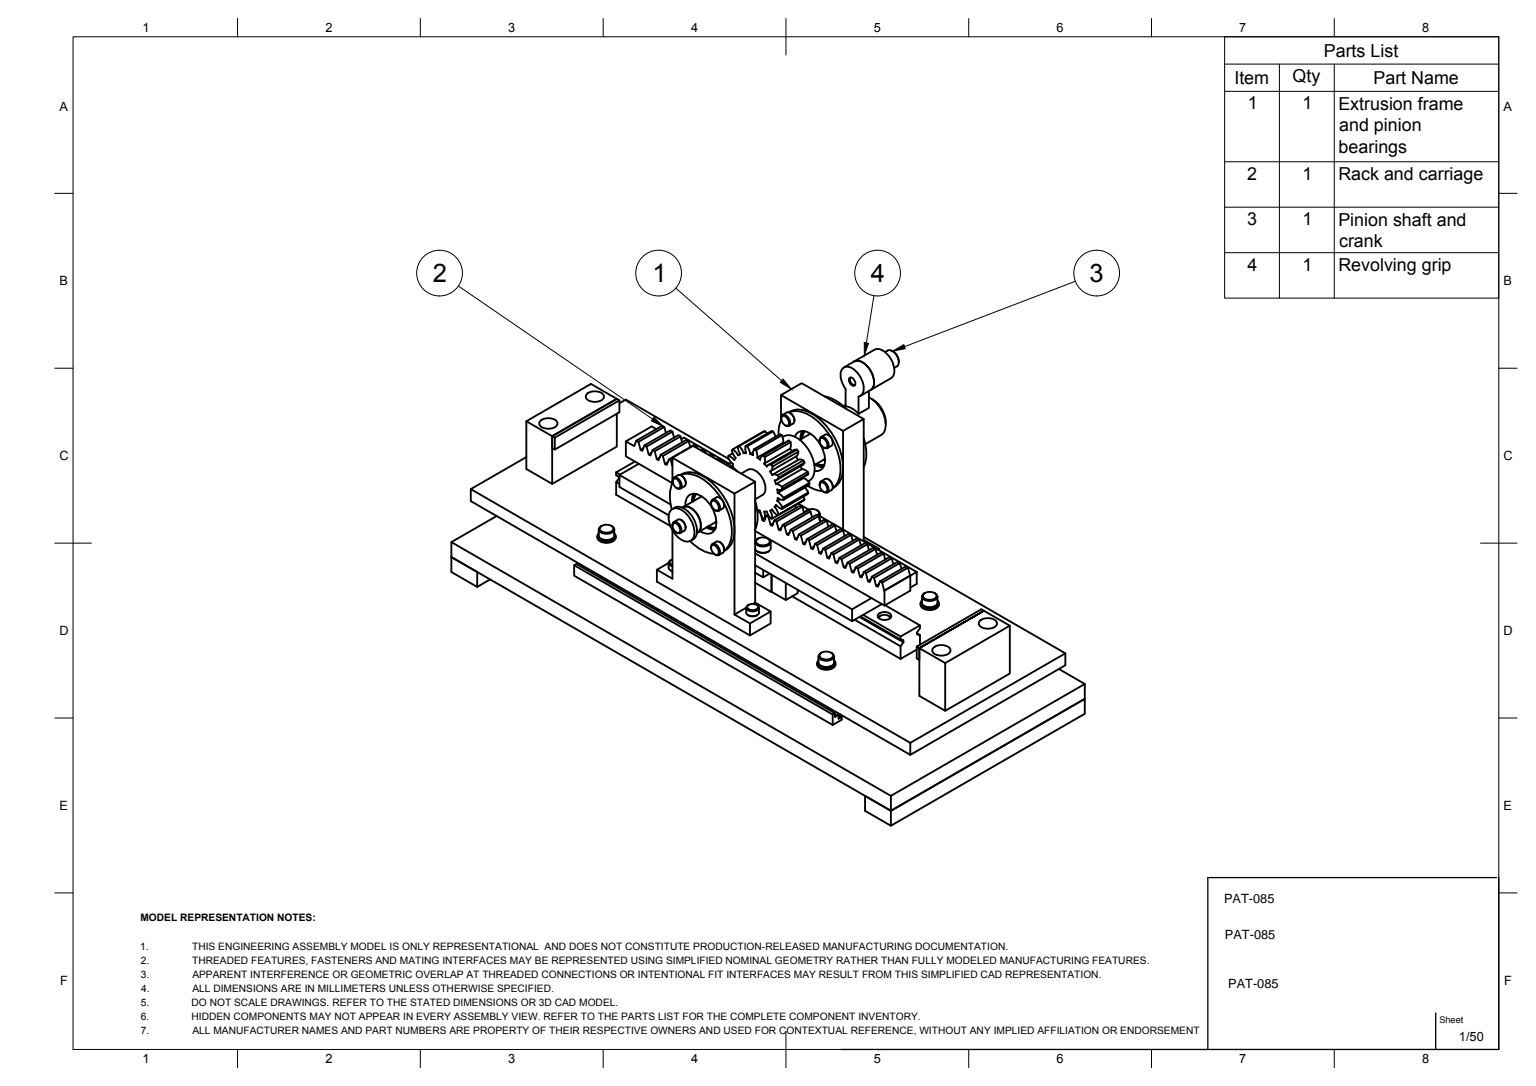
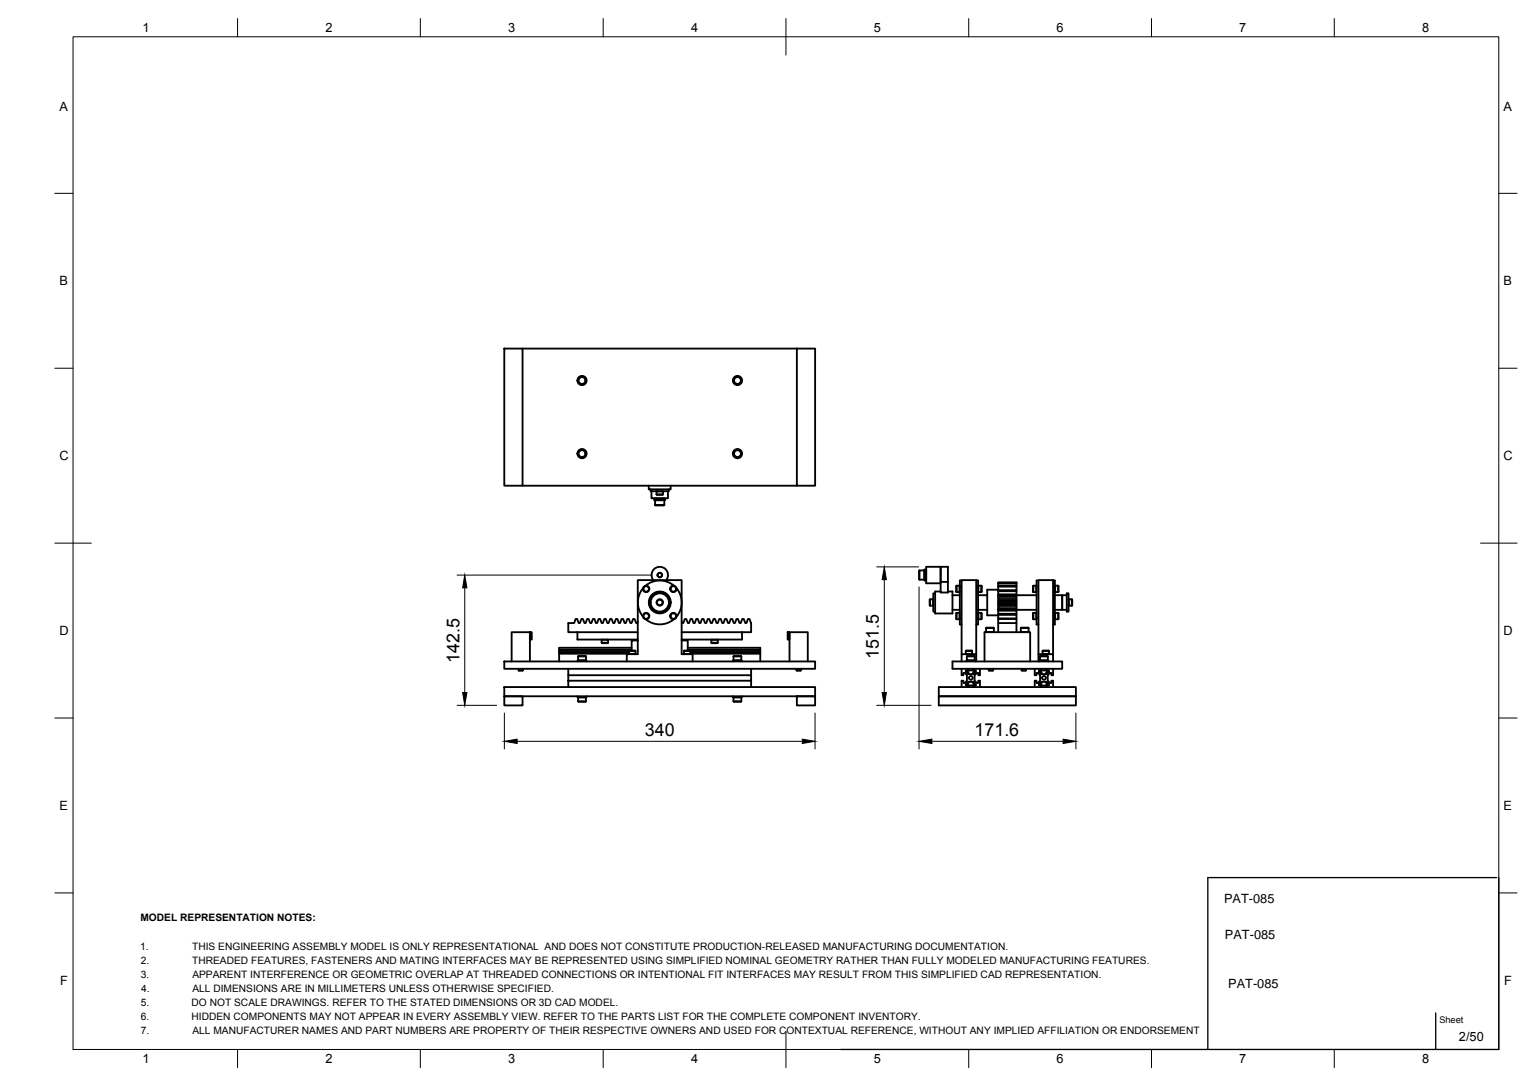
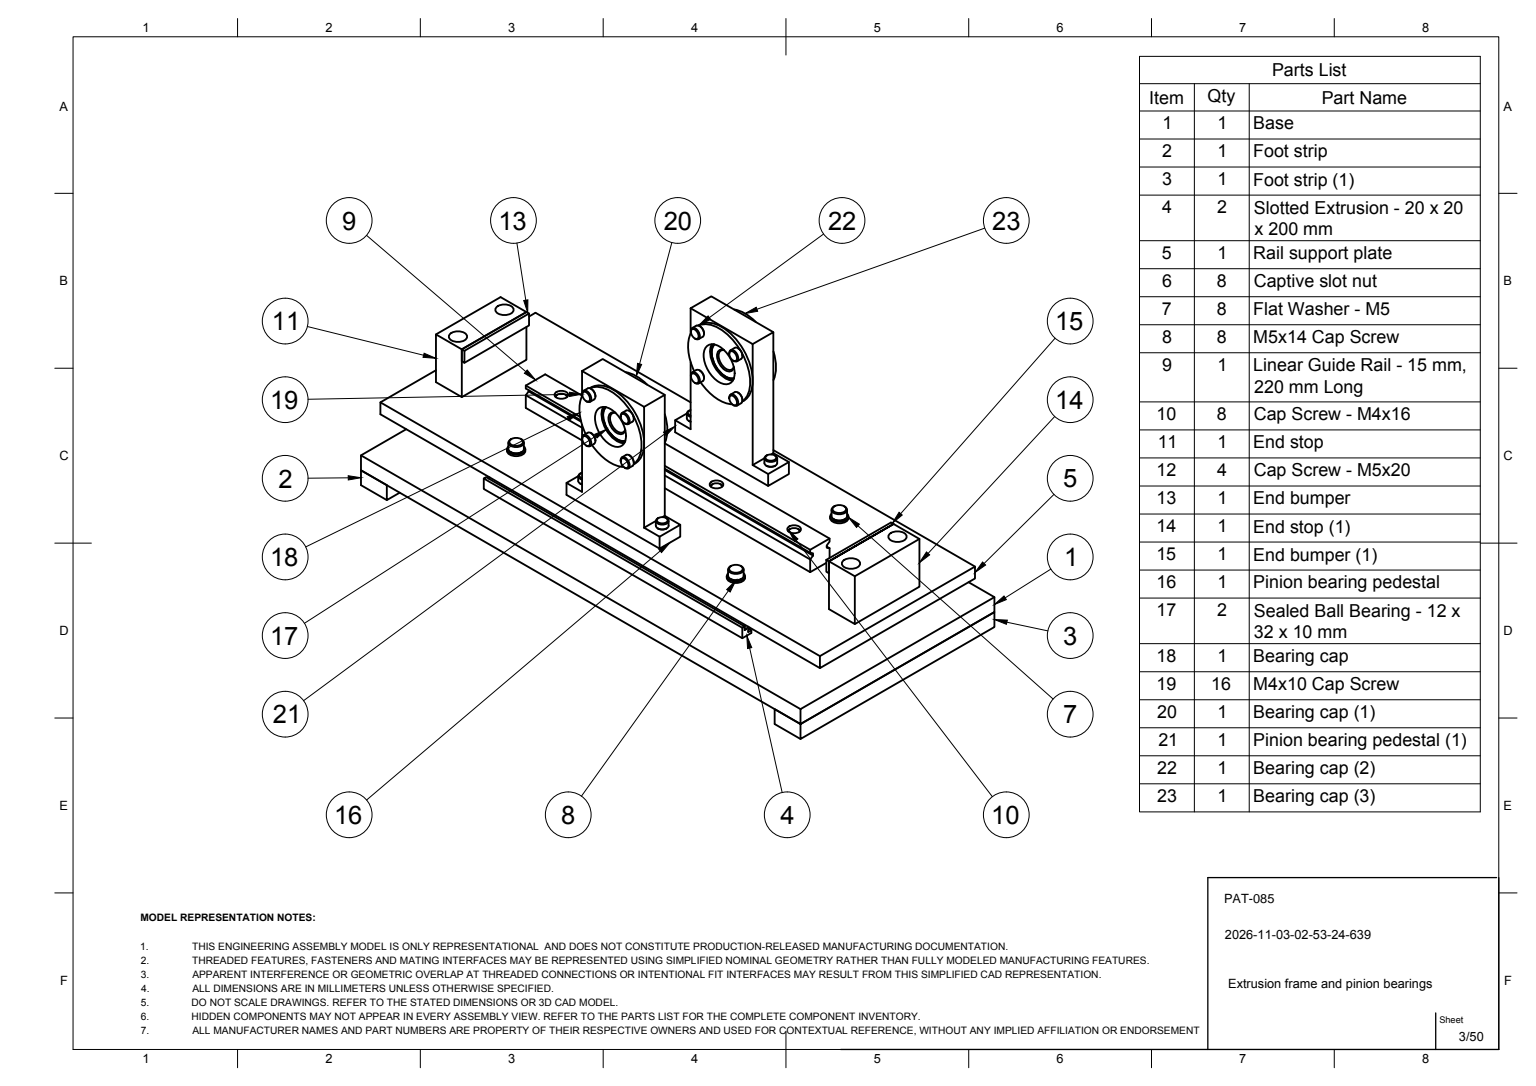
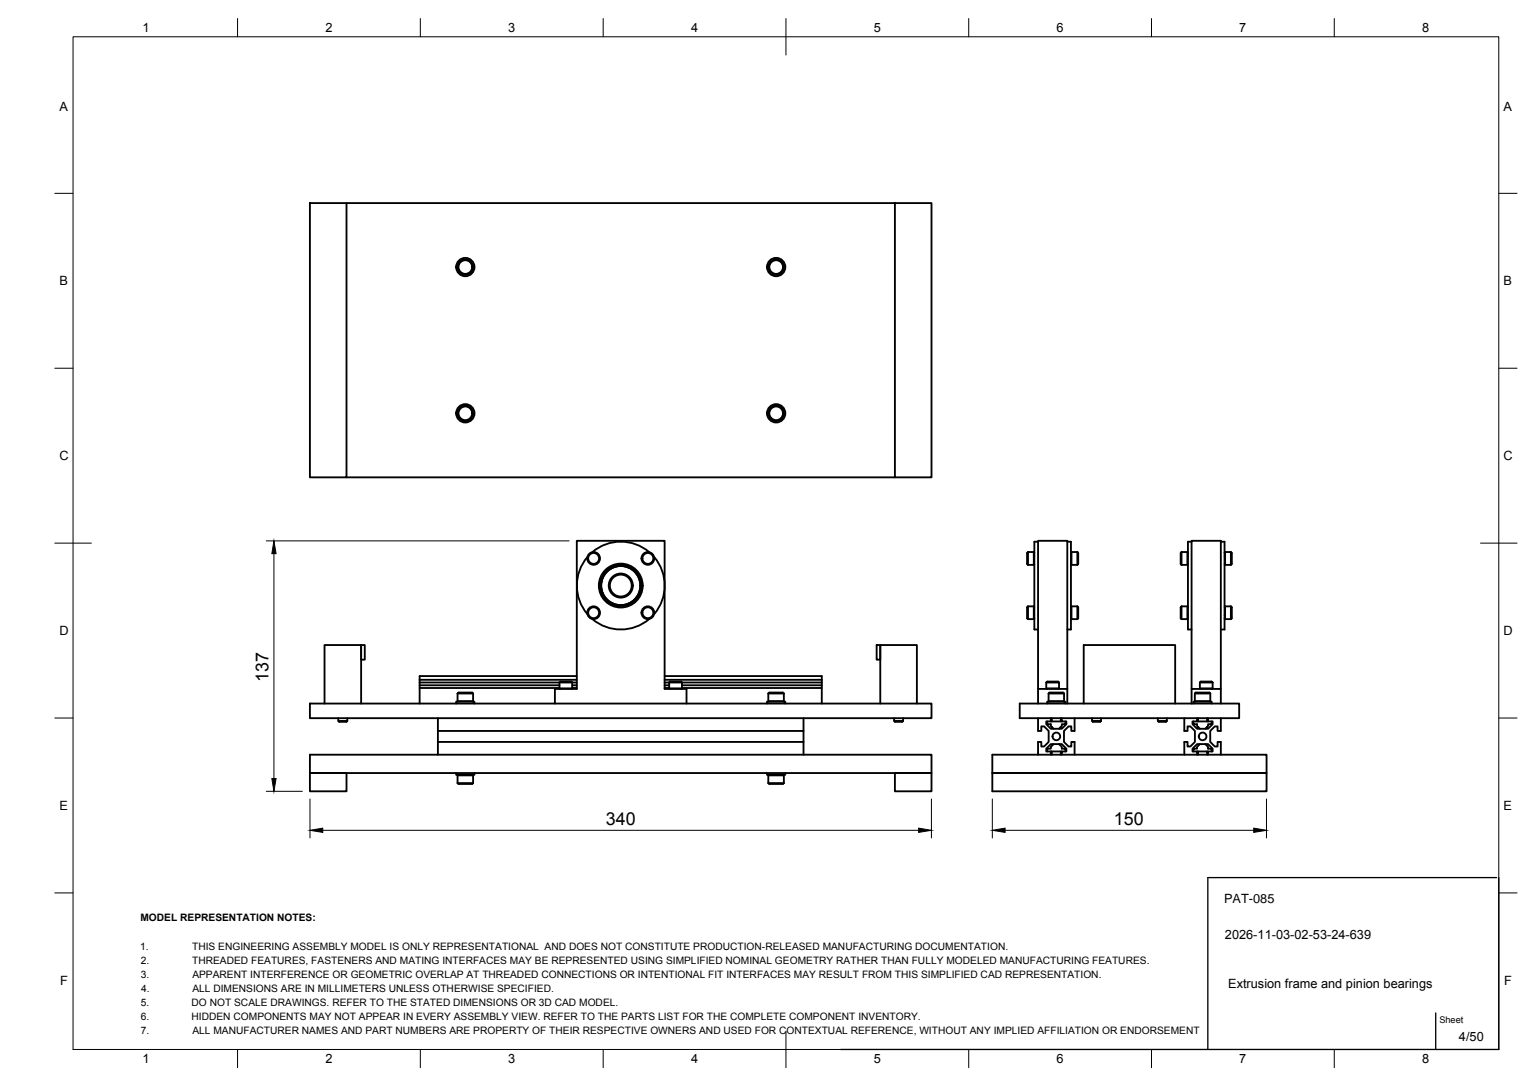
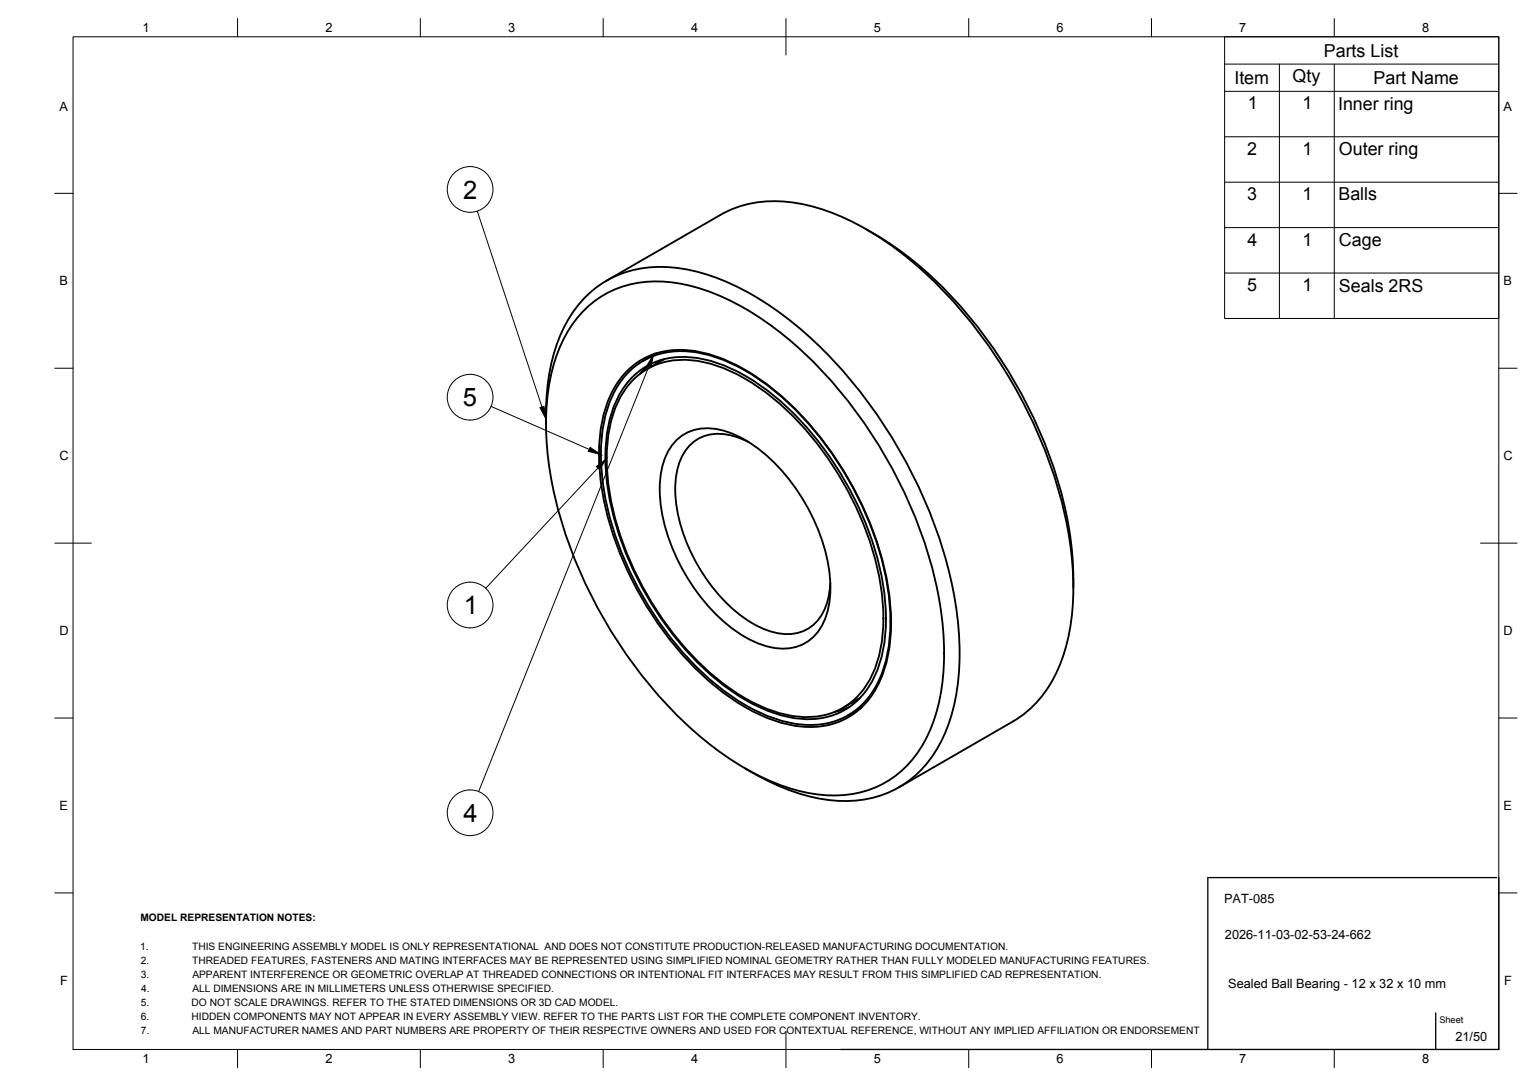
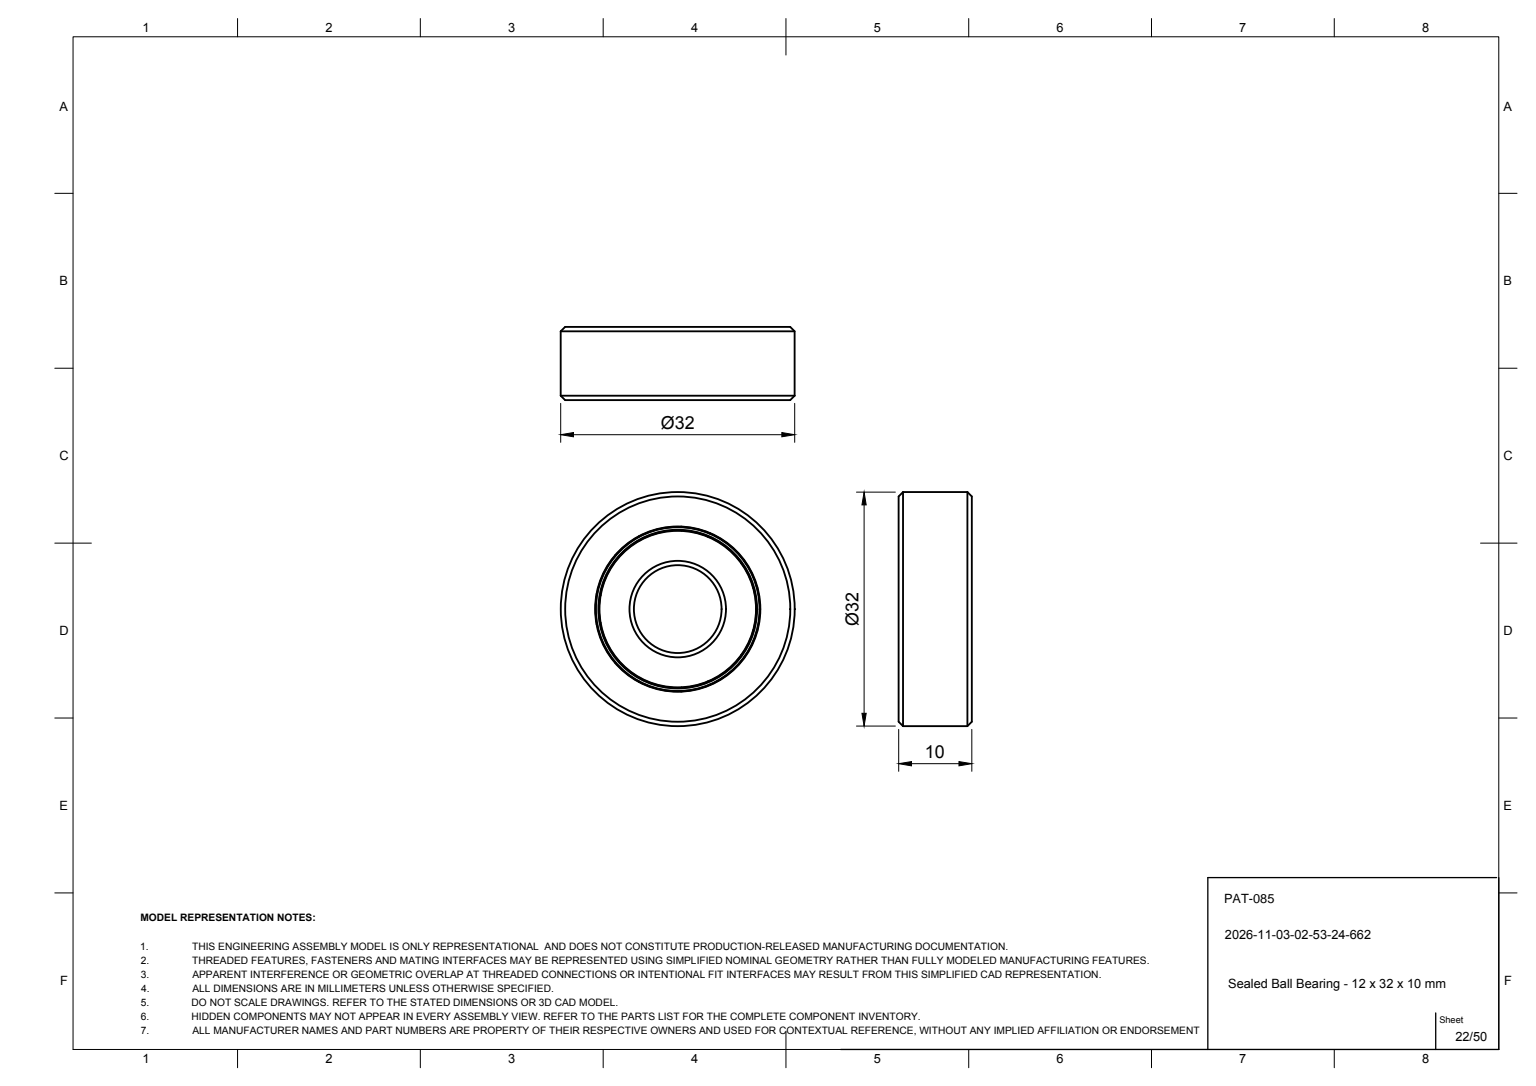
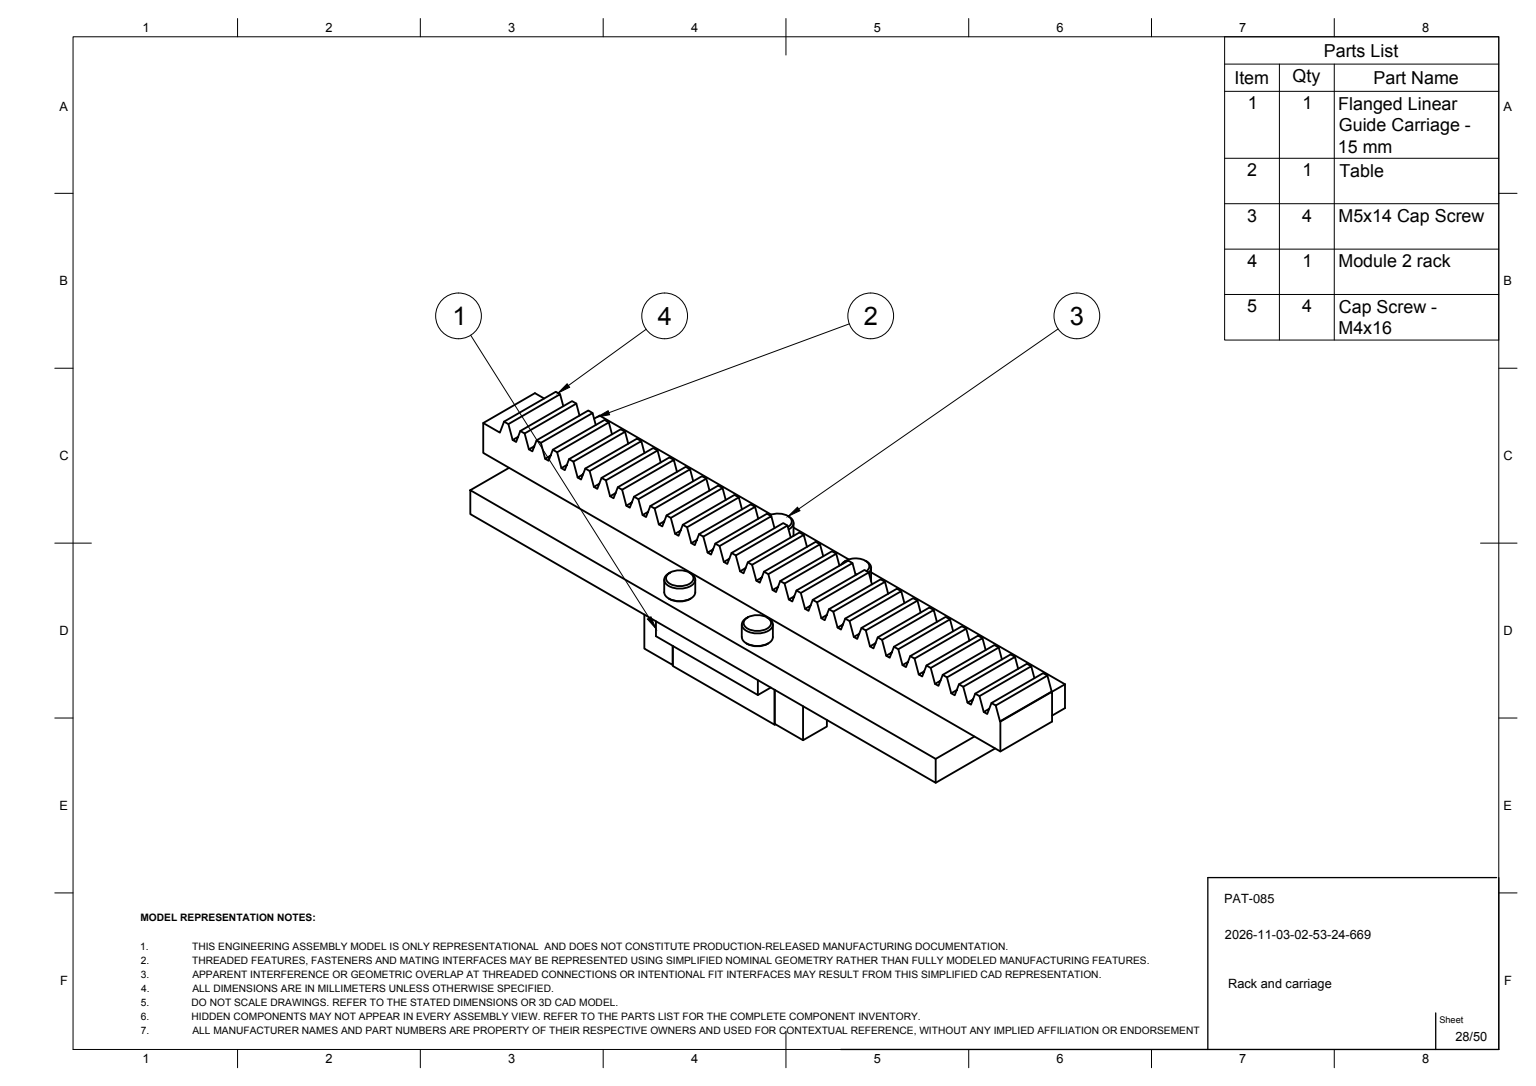
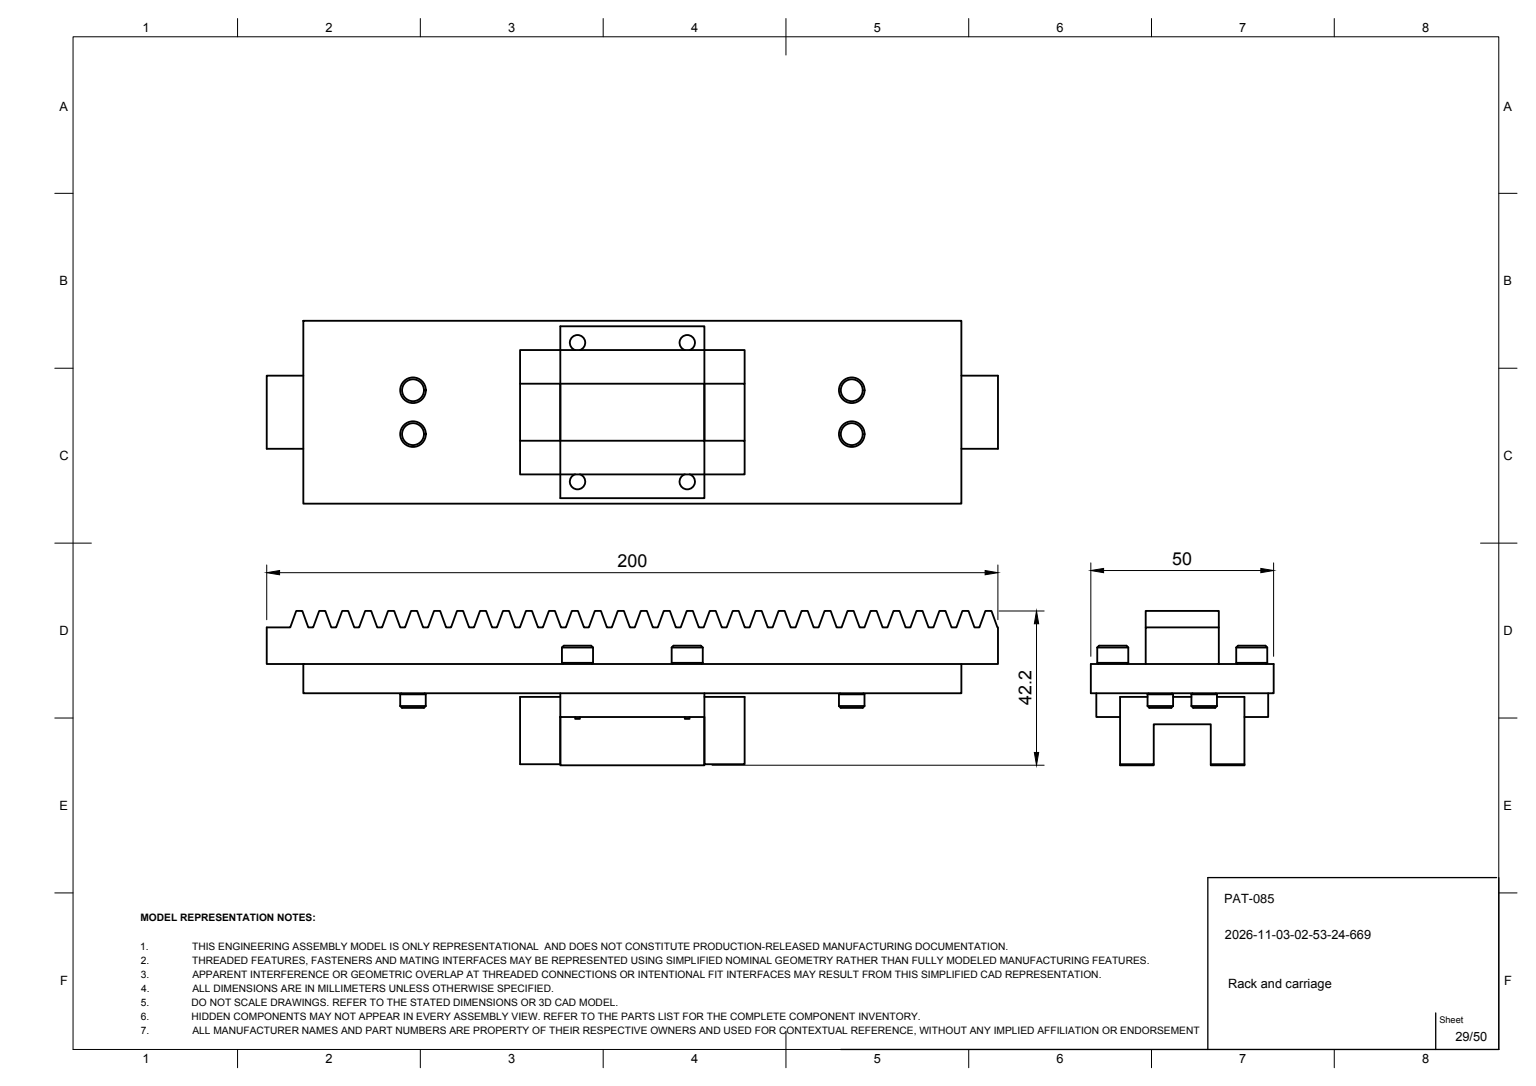
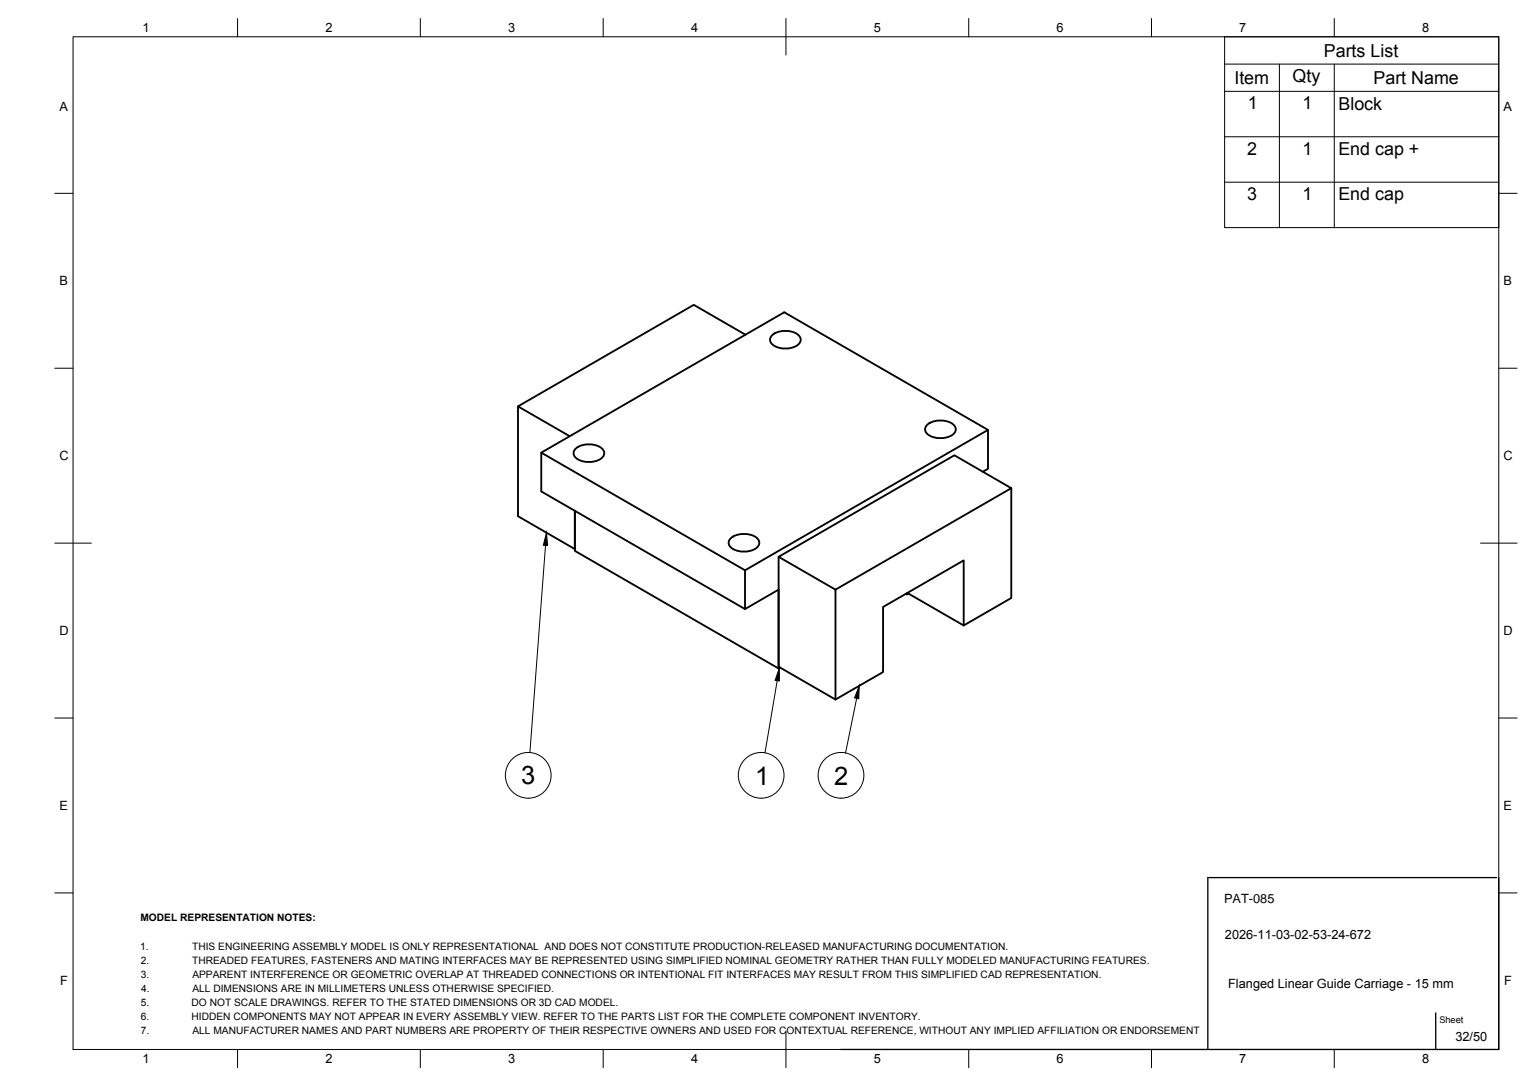
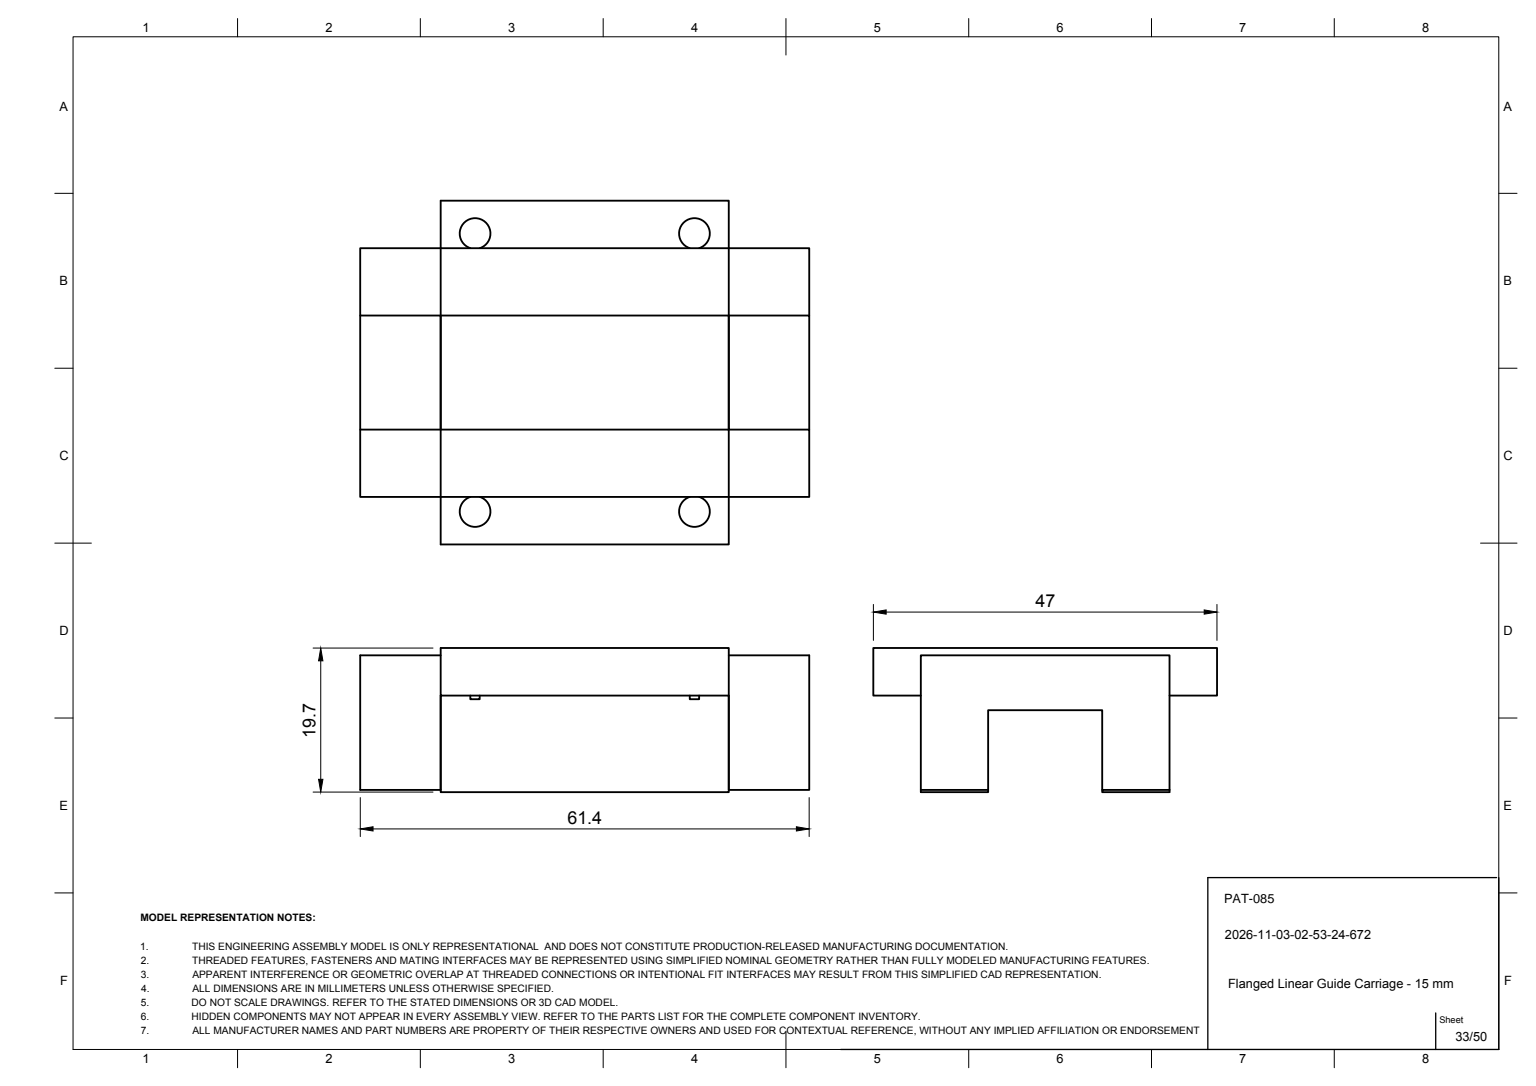
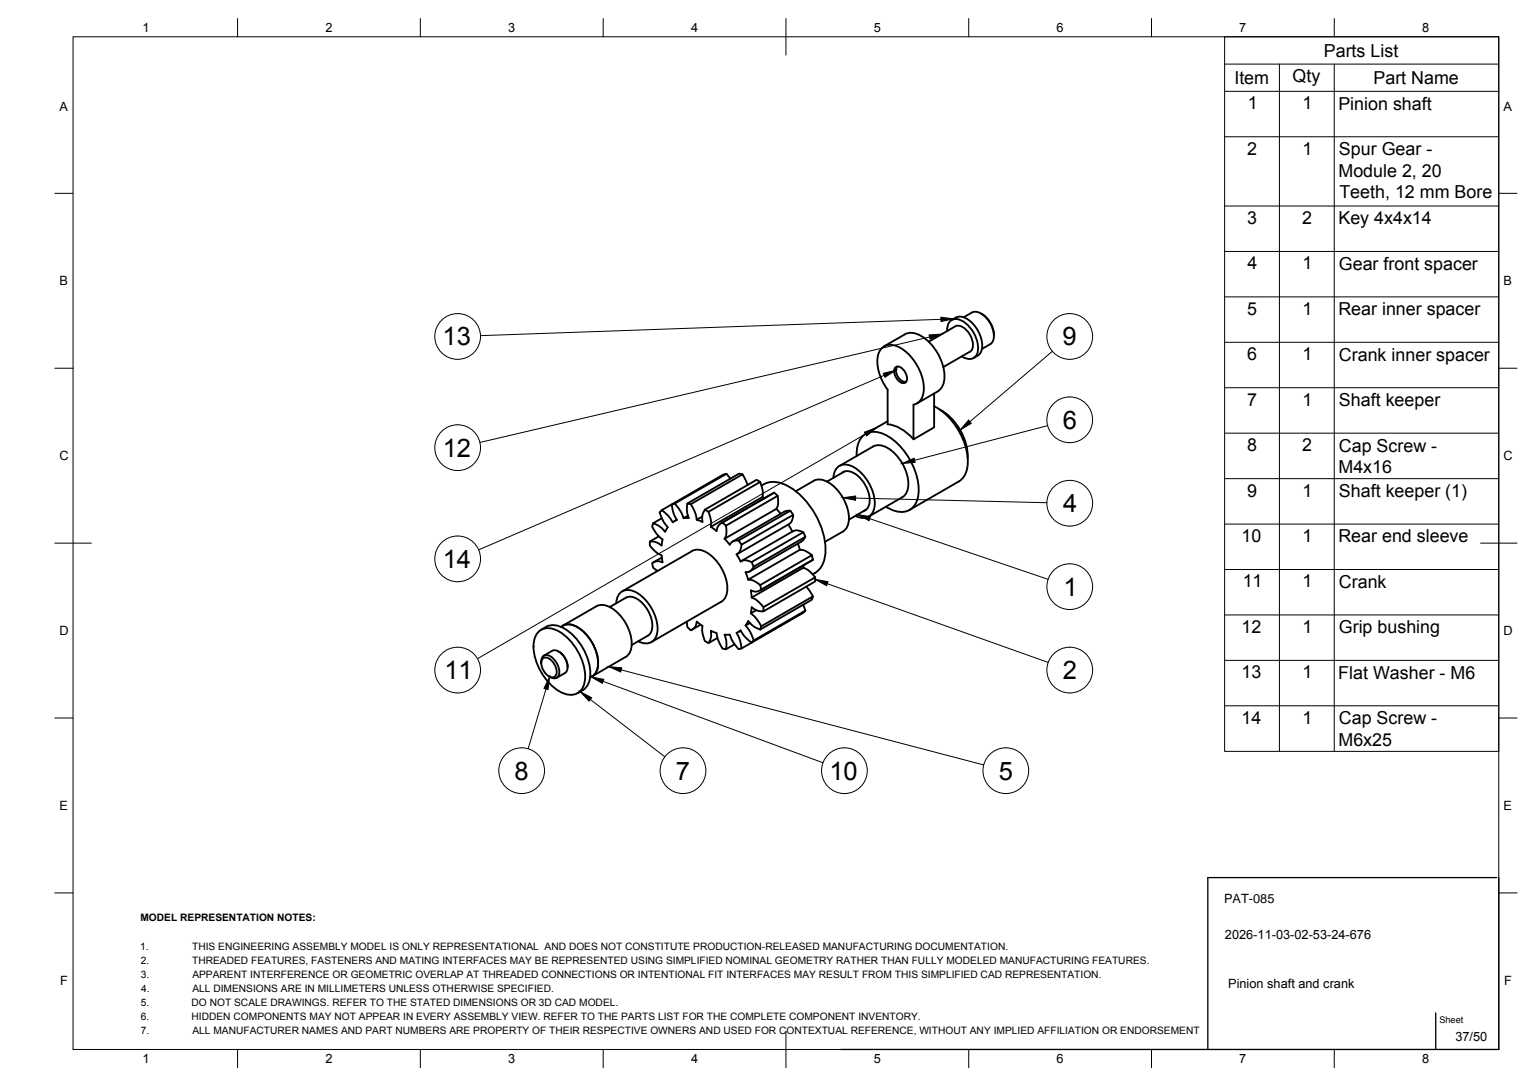
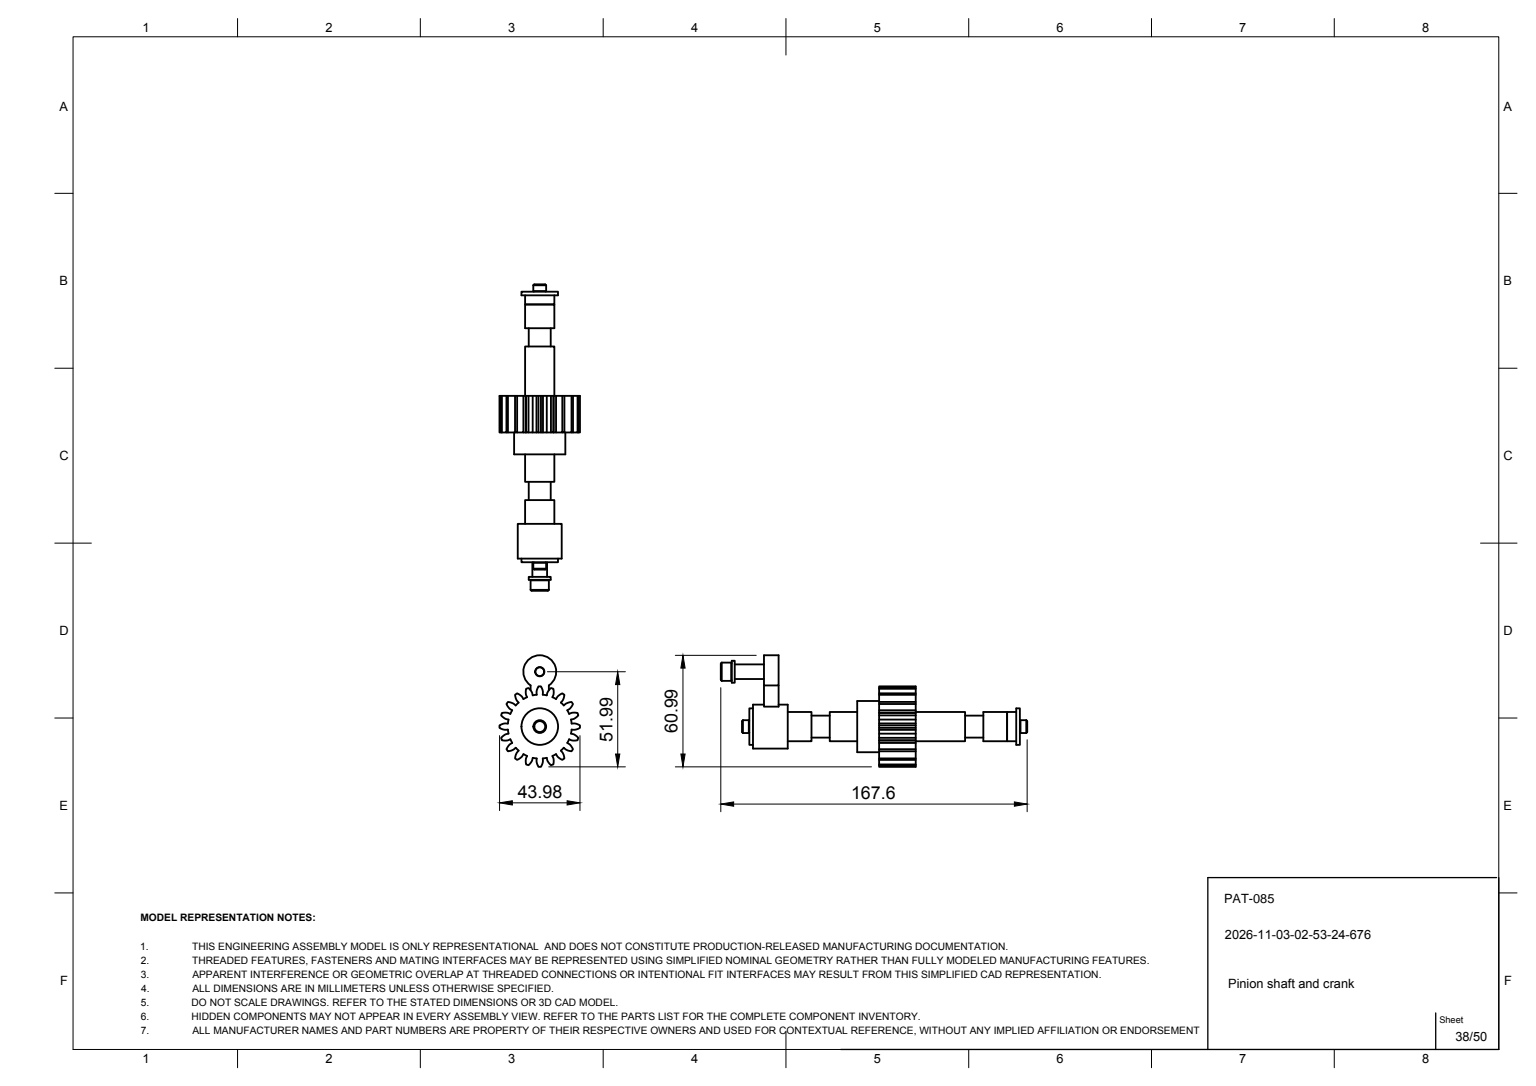
ISO-10303-21;
HEADER;
/* Generated by software containing ST-Developer
 * from STEP Tools, Inc. (www.steptools.com) 
 */

FILE_DESCRIPTION(
/* description */ ('Rack and pinion manual slide'),
/* implementation_level */ '2;1');

FILE_NAME(
/* name */ 'PAT-085',
/* time_stamp */ '2026-10-28T03:22:49-07:00',
/* author */ (''),
/* organization */ (''),
/* preprocessor_version */ 'ST-DEVELOPER v20.2',
/* originating_system */ 'Autodesk Translation Framework v15.17.0.0',
/* authorisation */ '');

FILE_SCHEMA (('AUTOMOTIVE_DESIGN { 1 0 10303 214 3 1 1 }'));
ENDSEC;

DATA;
#10=MECHANICAL_DESIGN_GEOMETRIC_PRESENTATION_REPRESENTATION('',(#732,#733,
#734,#735,#736,#737,#738,#739,#740,#741,#742,#743,#744,#745,#746,#747,#748,
#749,#750,#751,#752,#753,#754,#755,#756,#757,#758,#759,#760,#761,#762,#763,
#764,#765,#766,#767,#768,#769,#770,#771,#772,#773,#774,#775,#776,#777,#778,
#779,#780,#781,#782,#783,#784),#34851);
#11=(
BOUNDED_SURFACE()
B_SPLINE_SURFACE(5,1,((#25778,#25779),(#25780,#25781),(#25782,#25783),(#25784,
#25785),(#25786,#25787),(#25788,#25789),(#25790,#25791),(#25792,#25793),
(#25794,#25795),(#25796,#25797),(#25798,#25799),(#25800,#25801),(#25802,
#25803),(#25804,#25805),(#25806,#25807),(#25808,#25809),(#25810,#25811),
(#25812,#25813),(#25814,#25815),(#25816,#25817),(#25818,#25819),(#25820,
#25821),(#25822,#25823),(#25824,#25825),(#25826,#25827),(#25828,#25829),
(#25830,#25831),(#25832,#25833),(#25834,#25835),(#25836,#25837),(#25838,
#25839),(#25840,#25841),(#25842,#25843),(#25844,#25845),(#25846,#25847),
(#25848,#25849),(#25850,#25851),(#25852,#25853),(#25854,#25855),(#25856,
#25857),(#25858,#25859),(#25860,#25861),(#25862,#25863),(#25864,#25865),
(#25866,#25867),(#25868,#25869),(#25870,#25871),(#25872,#25873),(#25874,
#25875),(#25876,#25877),(#25878,#25879),(#25880,#25881),(#25882,#25883),
(#25884,#25885),(#25886,#25887),(#25888,#25889),(#25890,#25891),(#25892,
#25893),(#25894,#25895),(#25896,#25897),(#25898,#25899),(#25900,#25901),
(#25902,#25903),(#25904,#25905),(#25906,#25907),(#25908,#25909),(#25910,
#25911),(#25912,#25913),(#25914,#25915),(#25916,#25917)),.UNSPECIFIED.,
 .F.,.F.,.F.)
B_SPLINE_SURFACE_WITH_KNOTS((6,1,1,1,1,1,1,1,1,1,1,1,1,1,1,1,1,1,1,1,1,
1,1,1,1,1,1,1,1,1,1,1,1,1,1,1,1,1,1,1,1,1,1,1,1,1,1,1,1,1,1,1,1,1,1,1,1,
1,1,1,1,1,1,1,1,6),(2,2),(-1.,-0.984615384615383,-0.969230769230768,-0.953846153846152,
-0.938461538461537,-0.923076923076922,-0.907692307692306,-0.892307692307691,
-0.876923076923076,-0.86153846153846,-0.846153846153845,-0.83076923076923,
-0.815384615384614,-0.799999999999999,-0.784615384615384,-0.769230769230768,
-0.753846153846153,-0.738461538461538,-0.723076923076922,-0.707692307692307,
-0.692307692307692,-0.676923076923076,-0.661538461538461,-0.646153846153846,
-0.63076923076923,-0.615384615384615,-0.6,-0.584615384615384,-0.569230769230769,
-0.553846153846154,-0.538461538461538,-0.523076923076923,-0.507692307692308,
-0.492307692307692,-0.476923076923077,-0.461538461538462,-0.446153846153846,
-0.430769230769231,-0.415384615384615,-0.4,-0.384615384615385,-0.369230769230769,
-0.353846153846154,-0.338461538461538,-0.323076923076923,-0.307692307692308,
-0.292307692307692,-0.276923076923077,-0.261538461538462,-0.246153846153846,
-0.230769230769231,-0.215384615384615,-0.2,-0.184615384615385,-0.169230769230769,
-0.153846153846154,-0.138461538461538,-0.123076923076923,-0.107692307692308,
-0.0923076923076923,-0.0769230769230769,-0.0615384615384615,-0.0461538461538462,
-0.0307692307692308,-0.0153846153846154,0.),(-1.,1.),.UNSPECIFIED.)
GEOMETRIC_REPRESENTATION_ITEM()
RATIONAL_B_SPLINE_SURFACE(((1.,1.),(1.,1.),(1.,1.),(1.,1.),(1.,1.),(1.,
1.),(1.,1.),(1.,1.),(1.,1.),(1.,1.),(1.,1.),(1.,1.),(1.,1.),(1.,1.),(1.,
1.),(1.,1.),(1.,1.),(1.,1.),(1.,1.),(1.,1.),(1.,1.),(1.,1.),(1.,1.),(1.,
1.),(1.,1.),(1.,1.),(1.,1.),(1.,1.),(1.,1.),(1.,1.),(1.,1.),(1.,1.),(1.,
1.),(1.,1.),(1.,1.),(1.,1.),(1.,1.),(1.,1.),(1.,1.),(1.,1.),(1.,1.),(1.,
1.),(1.,1.),(1.,1.),(1.,1.),(1.,1.),(1.,1.),(1.,1.),(1.,1.),(1.,1.),(1.,
1.),(1.,1.),(1.,1.),(1.,1.),(1.,1.),(1.,1.),(1.,1.),(1.,1.),(1.,1.),(1.,
1.),(1.,1.),(1.,1.),(1.,1.),(1.,1.),(1.,1.),(1.,1.),(1.,1.),(1.,1.),(1.,
1.),(1.,1.)))
REPRESENTATION_ITEM('')
SURFACE()
);
#12=(
BOUNDED_SURFACE()
B_SPLINE_SURFACE(5,1,((#25996,#25997),(#25998,#25999),(#26000,#26001),(#26002,
#26003),(#26004,#26005),(#26006,#26007),(#26008,#26009),(#26010,#26011),
(#26012,#26013),(#26014,#26015),(#26016,#26017),(#26018,#26019),(#26020,
#26021),(#26022,#26023),(#26024,#26025),(#26026,#26027),(#26028,#26029),
(#26030,#26031),(#26032,#26033),(#26034,#26035),(#26036,#26037),(#26038,
#26039),(#26040,#26041),(#26042,#26043),(#26044,#26045),(#26046,#26047),
(#26048,#26049),(#26050,#26051),(#26052,#26053),(#26054,#26055),(#26056,
#26057),(#26058,#26059),(#26060,#26061),(#26062,#26063),(#26064,#26065),
(#26066,#26067),(#26068,#26069),(#26070,#26071),(#26072,#26073),(#26074,
#26075),(#26076,#26077),(#26078,#26079),(#26080,#26081),(#26082,#26083),
(#26084,#26085),(#26086,#26087),(#26088,#26089),(#26090,#26091),(#26092,
#26093),(#26094,#26095),(#26096,#26097),(#26098,#26099),(#26100,#26101),
(#26102,#26103),(#26104,#26105),(#26106,#26107),(#26108,#26109),(#26110,
#26111),(#26112,#26113),(#26114,#26115),(#26116,#26117),(#26118,#26119),
(#26120,#26121),(#26122,#26123),(#26124,#26125),(#26126,#26127),(#26128,
#26129),(#26130,#26131),(#26132,#26133),(#26134,#26135)),.UNSPECIFIED.,
 .F.,.F.,.F.)
B_SPLINE_SURFACE_WITH_KNOTS((6,1,1,1,1,1,1,1,1,1,1,1,1,1,1,1,1,1,1,1,1,
1,1,1,1,1,1,1,1,1,1,1,1,1,1,1,1,1,1,1,1,1,1,1,1,1,1,1,1,1,1,1,1,1,1,1,1,
1,1,1,1,1,1,1,1,6),(2,2),(-1.,-0.984615384615383,-0.969230769230768,-0.953846153846152,
-0.938461538461537,-0.923076923076922,-0.907692307692306,-0.892307692307691,
-0.876923076923076,-0.86153846153846,-0.846153846153845,-0.83076923076923,
-0.815384615384614,-0.799999999999999,-0.784615384615384,-0.769230769230768,
-0.753846153846153,-0.738461538461538,-0.723076923076922,-0.707692307692307,
-0.692307692307692,-0.676923076923076,-0.661538461538461,-0.646153846153846,
-0.63076923076923,-0.615384615384615,-0.6,-0.584615384615384,-0.569230769230769,
-0.553846153846154,-0.538461538461538,-0.523076923076923,-0.507692307692308,
-0.492307692307692,-0.476923076923077,-0.461538461538462,-0.446153846153846,
-0.430769230769231,-0.415384615384615,-0.4,-0.384615384615385,-0.369230769230769,
-0.353846153846154,-0.338461538461538,-0.323076923076923,-0.307692307692308,
-0.292307692307692,-0.276923076923077,-0.261538461538462,-0.246153846153846,
-0.230769230769231,-0.215384615384615,-0.2,-0.184615384615385,-0.169230769230769,
-0.153846153846154,-0.138461538461538,-0.123076923076923,-0.107692307692308,
-0.0923076923076923,-0.0769230769230769,-0.0615384615384615,-0.0461538461538462,
-0.0307692307692308,-0.0153846153846154,0.),(-1.,1.),.UNSPECIFIED.)
GEOMETRIC_REPRESENTATION_ITEM()
RATIONAL_B_SPLINE_SURFACE(((1.,1.),(1.,1.),(1.,1.),(1.,1.),(1.,1.),(1.,
1.),(1.,1.),(1.,1.),(1.,1.),(1.,1.),(1.,1.),(1.,1.),(1.,1.),(1.,1.),(1.,
1.),(1.,1.),(1.,1.),(1.,1.),(1.,1.),(1.,1.),(1.,1.),(1.,1.),(1.,1.),(1.,
1.),(1.,1.),(1.,1.),(1.,1.),(1.,1.),(1.,1.),(1.,1.),(1.,1.),(1.,1.),(1.,
1.),(1.,1.),(1.,1.),(1.,1.),(1.,1.),(1.,1.),(1.,1.),(1.,1.),(1.,1.),(1.,
1.),(1.,1.),(1.,1.),(1.,1.),(1.,1.),(1.,1.),(1.,1.),(1.,1.),(1.,1.),(1.,
1.),(1.,1.),(1.,1.),(1.,1.),(1.,1.),(1.,1.),(1.,1.),(1.,1.),(1.,1.),(1.,
1.),(1.,1.),(1.,1.),(1.,1.),(1.,1.),(1.,1.),(1.,1.),(1.,1.),(1.,1.),(1.,
1.),(1.,1.)))
REPRESENTATION_ITEM('')
SURFACE()
);
#13=(
BOUNDED_SURFACE()
B_SPLINE_SURFACE(5,1,((#26212,#26213),(#26214,#26215),(#26216,#26217),(#26218,
#26219),(#26220,#26221),(#26222,#26223),(#26224,#26225),(#26226,#26227),
(#26228,#26229),(#26230,#26231),(#26232,#26233),(#26234,#26235),(#26236,
#26237),(#26238,#26239),(#26240,#26241),(#26242,#26243),(#26244,#26245),
(#26246,#26247),(#26248,#26249),(#26250,#26251),(#26252,#26253),(#26254,
#26255),(#26256,#26257),(#26258,#26259),(#26260,#26261),(#26262,#26263),
(#26264,#26265),(#26266,#26267),(#26268,#26269),(#26270,#26271),(#26272,
#26273),(#26274,#26275),(#26276,#26277),(#26278,#26279),(#26280,#26281),
(#26282,#26283),(#26284,#26285),(#26286,#26287),(#26288,#26289),(#26290,
#26291),(#26292,#26293),(#26294,#26295),(#26296,#26297),(#26298,#26299),
(#26300,#26301),(#26302,#26303),(#26304,#26305),(#26306,#26307),(#26308,
#26309),(#26310,#26311),(#26312,#26313),(#26314,#26315),(#26316,#26317),
(#26318,#26319),(#26320,#26321),(#26322,#26323),(#26324,#26325),(#26326,
#26327),(#26328,#26329),(#26330,#26331),(#26332,#26333),(#26334,#26335),
(#26336,#26337),(#26338,#26339),(#26340,#26341),(#26342,#26343),(#26344,
#26345),(#26346,#26347),(#26348,#26349),(#26350,#26351)),.UNSPECIFIED.,
 .F.,.F.,.F.)
B_SPLINE_SURFACE_WITH_KNOTS((6,1,1,1,1,1,1,1,1,1,1,1,1,1,1,1,1,1,1,1,1,
1,1,1,1,1,1,1,1,1,1,1,1,1,1,1,1,1,1,1,1,1,1,1,1,1,1,1,1,1,1,1,1,1,1,1,1,
1,1,1,1,1,1,1,1,6),(2,2),(-1.,-0.984615384615383,-0.969230769230768,-0.953846153846152,
-0.938461538461537,-0.923076923076922,-0.907692307692306,-0.892307692307691,
-0.876923076923076,-0.86153846153846,-0.846153846153845,-0.83076923076923,
-0.815384615384614,-0.799999999999999,-0.784615384615384,-0.769230769230768,
-0.753846153846153,-0.738461538461538,-0.723076923076922,-0.707692307692307,
-0.692307692307692,-0.676923076923076,-0.661538461538461,-0.646153846153846,
-0.63076923076923,-0.615384615384615,-0.6,-0.584615384615384,-0.569230769230769,
-0.553846153846154,-0.538461538461538,-0.523076923076923,-0.507692307692308,
-0.492307692307692,-0.476923076923077,-0.461538461538462,-0.446153846153846,
-0.430769230769231,-0.415384615384615,-0.4,-0.384615384615385,-0.369230769230769,
-0.353846153846154,-0.338461538461538,-0.323076923076923,-0.307692307692308,
-0.292307692307692,-0.276923076923077,-0.261538461538462,-0.246153846153846,
-0.230769230769231,-0.215384615384615,-0.2,-0.184615384615385,-0.169230769230769,
-0.153846153846154,-0.138461538461538,-0.123076923076923,-0.107692307692308,
-0.0923076923076923,-0.0769230769230769,-0.0615384615384615,-0.0461538461538462,
-0.0307692307692308,-0.0153846153846154,0.),(-1.,1.),.UNSPECIFIED.)
GEOMETRIC_REPRESENTATION_ITEM()
RATIONAL_B_SPLINE_SURFACE(((1.,1.),(1.,1.),(1.,1.),(1.,1.),(1.,1.),(1.,
1.),(1.,1.),(1.,1.),(1.,1.),(1.,1.),(1.,1.),(1.,1.),(1.,1.),(1.,1.),(1.,
1.),(1.,1.),(1.,1.),(1.,1.),(1.,1.),(1.,1.),(1.,1.),(1.,1.),(1.,1.),(1.,
1.),(1.,1.),(1.,1.),(1.,1.),(1.,1.),(1.,1.),(1.,1.),(1.,1.),(1.,1.),(1.,
1.),(1.,1.),(1.,1.),(1.,1.),(1.,1.),(1.,1.),(1.,1.),(1.,1.),(1.,1.),(1.,
1.),(1.,1.),(1.,1.),(1.,1.),(1.,1.),(1.,1.),(1.,1.),(1.,1.),(1.,1.),(1.,
1.),(1.,1.),(1.,1.),(1.,1.),(1.,1.),(1.,1.),(1.,1.),(1.,1.),(1.,1.),(1.,
1.),(1.,1.),(1.,1.),(1.,1.),(1.,1.),(1.,1.),(1.,1.),(1.,1.),(1.,1.),(1.,
1.),(1.,1.)))
REPRESENTATION_ITEM('')
SURFACE()
);
#14=(
BOUNDED_SURFACE()
B_SPLINE_SURFACE(5,1,((#26428,#26429),(#26430,#26431),(#26432,#26433),(#26434,
#26435),(#26436,#26437),(#26438,#26439),(#26440,#26441),(#26442,#26443),
(#26444,#26445),(#26446,#26447),(#26448,#26449),(#26450,#26451),(#26452,
#26453),(#26454,#26455),(#26456,#26457),(#26458,#26459),(#26460,#26461),
(#26462,#26463),(#26464,#26465),(#26466,#26467),(#26468,#26469),(#26470,
#26471),(#26472,#26473),(#26474,#26475),(#26476,#26477),(#26478,#26479),
(#26480,#26481),(#26482,#26483),(#26484,#26485),(#26486,#26487),(#26488,
#26489),(#26490,#26491),(#26492,#26493),(#26494,#26495),(#26496,#26497),
(#26498,#26499),(#26500,#26501),(#26502,#26503),(#26504,#26505),(#26506,
#26507),(#26508,#26509),(#26510,#26511),(#26512,#26513),(#26514,#26515),
(#26516,#26517),(#26518,#26519),(#26520,#26521),(#26522,#26523),(#26524,
#26525),(#26526,#26527),(#26528,#26529),(#26530,#26531),(#26532,#26533),
(#26534,#26535),(#26536,#26537),(#26538,#26539),(#26540,#26541),(#26542,
#26543),(#26544,#26545),(#26546,#26547),(#26548,#26549),(#26550,#26551),
(#26552,#26553),(#26554,#26555),(#26556,#26557),(#26558,#26559),(#26560,
#26561),(#26562,#26563),(#26564,#26565),(#26566,#26567)),.UNSPECIFIED.,
 .F.,.F.,.F.)
B_SPLINE_SURFACE_WITH_KNOTS((6,1,1,1,1,1,1,1,1,1,1,1,1,1,1,1,1,1,1,1,1,
1,1,1,1,1,1,1,1,1,1,1,1,1,1,1,1,1,1,1,1,1,1,1,1,1,1,1,1,1,1,1,1,1,1,1,1,
1,1,1,1,1,1,1,1,6),(2,2),(-1.,-0.984615384615383,-0.969230769230768,-0.953846153846152,
-0.938461538461537,-0.923076923076922,-0.907692307692306,-0.892307692307691,
-0.876923076923076,-0.86153846153846,-0.846153846153845,-0.83076923076923,
-0.815384615384614,-0.799999999999999,-0.784615384615384,-0.769230769230768,
-0.753846153846153,-0.738461538461538,-0.723076923076922,-0.707692307692307,
-0.692307692307692,-0.676923076923076,-0.661538461538461,-0.646153846153846,
-0.63076923076923,-0.615384615384615,-0.6,-0.584615384615384,-0.569230769230769,
-0.553846153846154,-0.538461538461538,-0.523076923076923,-0.507692307692308,
-0.492307692307692,-0.476923076923077,-0.461538461538462,-0.446153846153846,
-0.430769230769231,-0.415384615384615,-0.4,-0.384615384615385,-0.369230769230769,
-0.353846153846154,-0.338461538461538,-0.323076923076923,-0.307692307692308,
-0.292307692307692,-0.276923076923077,-0.261538461538462,-0.246153846153846,
-0.230769230769231,-0.215384615384615,-0.2,-0.184615384615385,-0.169230769230769,
-0.153846153846154,-0.138461538461538,-0.123076923076923,-0.107692307692308,
-0.0923076923076923,-0.0769230769230769,-0.0615384615384615,-0.0461538461538462,
-0.0307692307692308,-0.0153846153846154,0.),(-1.,1.),.UNSPECIFIED.)
GEOMETRIC_REPRESENTATION_ITEM()
RATIONAL_B_SPLINE_SURFACE(((1.,1.),(1.,1.),(1.,1.),(1.,1.),(1.,1.),(1.,
1.),(1.,1.),(1.,1.),(1.,1.),(1.,1.),(1.,1.),(1.,1.),(1.,1.),(1.,1.),(1.,
1.),(1.,1.),(1.,1.),(1.,1.),(1.,1.),(1.,1.),(1.,1.),(1.,1.),(1.,1.),(1.,
1.),(1.,1.),(1.,1.),(1.,1.),(1.,1.),(1.,1.),(1.,1.),(1.,1.),(1.,1.),(1.,
1.),(1.,1.),(1.,1.),(1.,1.),(1.,1.),(1.,1.),(1.,1.),(1.,1.),(1.,1.),(1.,
1.),(1.,1.),(1.,1.),(1.,1.),(1.,1.),(1.,1.),(1.,1.),(1.,1.),(1.,1.),(1.,
1.),(1.,1.),(1.,1.),(1.,1.),(1.,1.),(1.,1.),(1.,1.),(1.,1.),(1.,1.),(1.,
1.),(1.,1.),(1.,1.),(1.,1.),(1.,1.),(1.,1.),(1.,1.),(1.,1.),(1.,1.),(1.,
1.),(1.,1.)))
REPRESENTATION_ITEM('')
SURFACE()
);
#15=(
BOUNDED_SURFACE()
B_SPLINE_SURFACE(5,1,((#26644,#26645),(#26646,#26647),(#26648,#26649),(#26650,
#26651),(#26652,#26653),(#26654,#26655),(#26656,#26657),(#26658,#26659),
(#26660,#26661),(#26662,#26663),(#26664,#26665),(#26666,#26667),(#26668,
#26669),(#26670,#26671),(#26672,#26673),(#26674,#26675),(#26676,#26677),
(#26678,#26679),(#26680,#26681),(#26682,#26683),(#26684,#26685),(#26686,
#26687),(#26688,#26689),(#26690,#26691),(#26692,#26693),(#26694,#26695),
(#26696,#26697),(#26698,#26699),(#26700,#26701),(#26702,#26703),(#26704,
#26705),(#26706,#26707),(#26708,#26709),(#26710,#26711),(#26712,#26713),
(#26714,#26715),(#26716,#26717),(#26718,#26719),(#26720,#26721),(#26722,
#26723),(#26724,#26725),(#26726,#26727),(#26728,#26729),(#26730,#26731),
(#26732,#26733),(#26734,#26735),(#26736,#26737),(#26738,#26739),(#26740,
#26741),(#26742,#26743),(#26744,#26745),(#26746,#26747),(#26748,#26749),
(#26750,#26751),(#26752,#26753),(#26754,#26755),(#26756,#26757),(#26758,
#26759),(#26760,#26761),(#26762,#26763),(#26764,#26765),(#26766,#26767),
(#26768,#26769),(#26770,#26771),(#26772,#26773),(#26774,#26775),(#26776,
#26777),(#26778,#26779),(#26780,#26781),(#26782,#26783)),.UNSPECIFIED.,
 .F.,.F.,.F.)
B_SPLINE_SURFACE_WITH_KNOTS((6,1,1,1,1,1,1,1,1,1,1,1,1,1,1,1,1,1,1,1,1,
1,1,1,1,1,1,1,1,1,1,1,1,1,1,1,1,1,1,1,1,1,1,1,1,1,1,1,1,1,1,1,1,1,1,1,1,
1,1,1,1,1,1,1,1,6),(2,2),(-1.,-0.984615384615383,-0.969230769230768,-0.953846153846152,
-0.938461538461537,-0.923076923076922,-0.907692307692306,-0.892307692307691,
-0.876923076923076,-0.86153846153846,-0.846153846153845,-0.83076923076923,
-0.815384615384614,-0.799999999999999,-0.784615384615384,-0.769230769230768,
-0.753846153846153,-0.738461538461538,-0.723076923076922,-0.707692307692307,
-0.692307692307692,-0.676923076923076,-0.661538461538461,-0.646153846153846,
-0.63076923076923,-0.615384615384615,-0.6,-0.584615384615384,-0.569230769230769,
-0.553846153846154,-0.538461538461538,-0.523076923076923,-0.507692307692308,
-0.492307692307692,-0.476923076923077,-0.461538461538462,-0.446153846153846,
-0.430769230769231,-0.415384615384615,-0.4,-0.384615384615385,-0.369230769230769,
-0.353846153846154,-0.338461538461538,-0.323076923076923,-0.307692307692308,
-0.292307692307692,-0.276923076923077,-0.261538461538462,-0.246153846153846,
-0.230769230769231,-0.215384615384615,-0.2,-0.184615384615385,-0.169230769230769,
-0.153846153846154,-0.138461538461538,-0.123076923076923,-0.107692307692308,
-0.0923076923076923,-0.0769230769230769,-0.0615384615384615,-0.0461538461538462,
-0.0307692307692308,-0.0153846153846154,0.),(-1.,1.),.UNSPECIFIED.)
GEOMETRIC_REPRESENTATION_ITEM()
RATIONAL_B_SPLINE_SURFACE(((1.,1.),(1.,1.),(1.,1.),(1.,1.),(1.,1.),(1.,
1.),(1.,1.),(1.,1.),(1.,1.),(1.,1.),(1.,1.),(1.,1.),(1.,1.),(1.,1.),(1.,
1.),(1.,1.),(1.,1.),(1.,1.),(1.,1.),(1.,1.),(1.,1.),(1.,1.),(1.,1.),(1.,
1.),(1.,1.),(1.,1.),(1.,1.),(1.,1.),(1.,1.),(1.,1.),(1.,1.),(1.,1.),(1.,
1.),(1.,1.),(1.,1.),(1.,1.),(1.,1.),(1.,1.),(1.,1.),(1.,1.),(1.,1.),(1.,
1.),(1.,1.),(1.,1.),(1.,1.),(1.,1.),(1.,1.),(1.,1.),(1.,1.),(1.,1.),(1.,
1.),(1.,1.),(1.,1.),(1.,1.),(1.,1.),(1.,1.),(1.,1.),(1.,1.),(1.,1.),(1.,
1.),(1.,1.),(1.,1.),(1.,1.),(1.,1.),(1.,1.),(1.,1.),(1.,1.),(1.,1.),(1.,
1.),(1.,1.)))
REPRESENTATION_ITEM('')
SURFACE()
);
#16=(
BOUNDED_SURFACE()
B_SPLINE_SURFACE(5,1,((#26860,#26861),(#26862,#26863),(#26864,#26865),(#26866,
#26867),(#26868,#26869),(#26870,#26871),(#26872,#26873),(#26874,#26875),
(#26876,#26877),(#26878,#26879),(#26880,#26881),(#26882,#26883),(#26884,
#26885),(#26886,#26887),(#26888,#26889),(#26890,#26891),(#26892,#26893),
(#26894,#26895),(#26896,#26897),(#26898,#26899),(#26900,#26901),(#26902,
#26903),(#26904,#26905),(#26906,#26907),(#26908,#26909),(#26910,#26911),
(#26912,#26913),(#26914,#26915),(#26916,#26917),(#26918,#26919),(#26920,
#26921),(#26922,#26923),(#26924,#26925),(#26926,#26927),(#26928,#26929),
(#26930,#26931),(#26932,#26933),(#26934,#26935),(#26936,#26937),(#26938,
#26939),(#26940,#26941),(#26942,#26943),(#26944,#26945),(#26946,#26947),
(#26948,#26949),(#26950,#26951),(#26952,#26953),(#26954,#26955),(#26956,
#26957),(#26958,#26959),(#26960,#26961),(#26962,#26963),(#26964,#26965),
(#26966,#26967),(#26968,#26969),(#26970,#26971),(#26972,#26973),(#26974,
#26975),(#26976,#26977),(#26978,#26979),(#26980,#26981),(#26982,#26983),
(#26984,#26985),(#26986,#26987),(#26988,#26989),(#26990,#26991),(#26992,
#26993),(#26994,#26995),(#26996,#26997),(#26998,#26999)),.UNSPECIFIED.,
 .F.,.F.,.F.)
B_SPLINE_SURFACE_WITH_KNOTS((6,1,1,1,1,1,1,1,1,1,1,1,1,1,1,1,1,1,1,1,1,
1,1,1,1,1,1,1,1,1,1,1,1,1,1,1,1,1,1,1,1,1,1,1,1,1,1,1,1,1,1,1,1,1,1,1,1,
1,1,1,1,1,1,1,1,6),(2,2),(-1.,-0.984615384615383,-0.969230769230768,-0.953846153846152,
-0.938461538461537,-0.923076923076922,-0.907692307692306,-0.892307692307691,
-0.876923076923076,-0.86153846153846,-0.846153846153845,-0.83076923076923,
-0.815384615384614,-0.799999999999999,-0.784615384615384,-0.769230769230768,
-0.753846153846153,-0.738461538461538,-0.723076923076922,-0.707692307692307,
-0.692307692307692,-0.676923076923076,-0.661538461538461,-0.646153846153846,
-0.63076923076923,-0.615384615384615,-0.6,-0.584615384615384,-0.569230769230769,
-0.553846153846154,-0.538461538461538,-0.523076923076923,-0.507692307692308,
-0.492307692307692,-0.476923076923077,-0.461538461538462,-0.446153846153846,
-0.430769230769231,-0.415384615384615,-0.4,-0.384615384615385,-0.369230769230769,
-0.353846153846154,-0.338461538461538,-0.323076923076923,-0.307692307692308,
-0.292307692307692,-0.276923076923077,-0.261538461538462,-0.246153846153846,
-0.230769230769231,-0.215384615384615,-0.2,-0.184615384615385,-0.169230769230769,
-0.153846153846154,-0.138461538461538,-0.123076923076923,-0.107692307692308,
-0.0923076923076923,-0.0769230769230769,-0.0615384615384615,-0.0461538461538462,
-0.0307692307692308,-0.0153846153846154,0.),(-1.,1.),.UNSPECIFIED.)
GEOMETRIC_REPRESENTATION_ITEM()
RATIONAL_B_SPLINE_SURFACE(((1.,1.),(1.,1.),(1.,1.),(1.,1.),(1.,1.),(1.,
1.),(1.,1.),(1.,1.),(1.,1.),(1.,1.),(1.,1.),(1.,1.),(1.,1.),(1.,1.),(1.,
1.),(1.,1.),(1.,1.),(1.,1.),(1.,1.),(1.,1.),(1.,1.),(1.,1.),(1.,1.),(1.,
1.),(1.,1.),(1.,1.),(1.,1.),(1.,1.),(1.,1.),(1.,1.),(1.,1.),(1.,1.),(1.,
1.),(1.,1.),(1.,1.),(1.,1.),(1.,1.),(1.,1.),(1.,1.),(1.,1.),(1.,1.),(1.,
1.),(1.,1.),(1.,1.),(1.,1.),(1.,1.),(1.,1.),(1.,1.),(1.,1.),(1.,1.),(1.,
1.),(1.,1.),(1.,1.),(1.,1.),(1.,1.),(1.,1.),(1.,1.),(1.,1.),(1.,1.),(1.,
1.),(1.,1.),(1.,1.),(1.,1.),(1.,1.),(1.,1.),(1.,1.),(1.,1.),(1.,1.),(1.,
1.),(1.,1.)))
REPRESENTATION_ITEM('')
SURFACE()
);
#17=(
BOUNDED_SURFACE()
B_SPLINE_SURFACE(5,1,((#27076,#27077),(#27078,#27079),(#27080,#27081),(#27082,
#27083),(#27084,#27085),(#27086,#27087),(#27088,#27089),(#27090,#27091),
(#27092,#27093),(#27094,#27095),(#27096,#27097),(#27098,#27099),(#27100,
#27101),(#27102,#27103),(#27104,#27105),(#27106,#27107),(#27108,#27109),
(#27110,#27111),(#27112,#27113),(#27114,#27115),(#27116,#27117),(#27118,
#27119),(#27120,#27121),(#27122,#27123),(#27124,#27125),(#27126,#27127),
(#27128,#27129),(#27130,#27131),(#27132,#27133),(#27134,#27135),(#27136,
#27137),(#27138,#27139),(#27140,#27141),(#27142,#27143),(#27144,#27145),
(#27146,#27147),(#27148,#27149),(#27150,#27151),(#27152,#27153),(#27154,
#27155),(#27156,#27157),(#27158,#27159),(#27160,#27161),(#27162,#27163),
(#27164,#27165),(#27166,#27167),(#27168,#27169),(#27170,#27171),(#27172,
#27173),(#27174,#27175),(#27176,#27177),(#27178,#27179),(#27180,#27181),
(#27182,#27183),(#27184,#27185),(#27186,#27187),(#27188,#27189),(#27190,
#27191),(#27192,#27193),(#27194,#27195),(#27196,#27197),(#27198,#27199),
(#27200,#27201),(#27202,#27203),(#27204,#27205),(#27206,#27207),(#27208,
#27209),(#27210,#27211),(#27212,#27213),(#27214,#27215)),.UNSPECIFIED.,
 .F.,.F.,.F.)
B_SPLINE_SURFACE_WITH_KNOTS((6,1,1,1,1,1,1,1,1,1,1,1,1,1,1,1,1,1,1,1,1,
1,1,1,1,1,1,1,1,1,1,1,1,1,1,1,1,1,1,1,1,1,1,1,1,1,1,1,1,1,1,1,1,1,1,1,1,
1,1,1,1,1,1,1,1,6),(2,2),(-1.,-0.984615384615383,-0.969230769230768,-0.953846153846152,
-0.938461538461537,-0.923076923076922,-0.907692307692306,-0.892307692307691,
-0.876923076923076,-0.86153846153846,-0.846153846153845,-0.83076923076923,
-0.815384615384614,-0.799999999999999,-0.784615384615384,-0.769230769230768,
-0.753846153846153,-0.738461538461538,-0.723076923076922,-0.707692307692307,
-0.692307692307692,-0.676923076923076,-0.661538461538461,-0.646153846153846,
-0.63076923076923,-0.615384615384615,-0.6,-0.584615384615384,-0.569230769230769,
-0.553846153846154,-0.538461538461538,-0.523076923076923,-0.507692307692308,
-0.492307692307692,-0.476923076923077,-0.461538461538462,-0.446153846153846,
-0.430769230769231,-0.415384615384615,-0.4,-0.384615384615385,-0.369230769230769,
-0.353846153846154,-0.338461538461538,-0.323076923076923,-0.307692307692308,
-0.292307692307692,-0.276923076923077,-0.261538461538462,-0.246153846153846,
-0.230769230769231,-0.215384615384615,-0.2,-0.184615384615385,-0.169230769230769,
-0.153846153846154,-0.138461538461538,-0.123076923076923,-0.107692307692308,
-0.0923076923076923,-0.0769230769230769,-0.0615384615384615,-0.0461538461538462,
-0.0307692307692308,-0.0153846153846154,0.),(-1.,1.),.UNSPECIFIED.)
GEOMETRIC_REPRESENTATION_ITEM()
RATIONAL_B_SPLINE_SURFACE(((1.,1.),(1.,1.),(1.,1.),(1.,1.),(1.,1.),(1.,
1.),(1.,1.),(1.,1.),(1.,1.),(1.,1.),(1.,1.),(1.,1.),(1.,1.),(1.,1.),(1.,
1.),(1.,1.),(1.,1.),(1.,1.),(1.,1.),(1.,1.),(1.,1.),(1.,1.),(1.,1.),(1.,
1.),(1.,1.),(1.,1.),(1.,1.),(1.,1.),(1.,1.),(1.,1.),(1.,1.),(1.,1.),(1.,
1.),(1.,1.),(1.,1.),(1.,1.),(1.,1.),(1.,1.),(1.,1.),(1.,1.),(1.,1.),(1.,
1.),(1.,1.),(1.,1.),(1.,1.),(1.,1.),(1.,1.),(1.,1.),(1.,1.),(1.,1.),(1.,
1.),(1.,1.),(1.,1.),(1.,1.),(1.,1.),(1.,1.),(1.,1.),(1.,1.),(1.,1.),(1.,
1.),(1.,1.),(1.,1.),(1.,1.),(1.,1.),(1.,1.),(1.,1.),(1.,1.),(1.,1.),(1.,
1.),(1.,1.)))
REPRESENTATION_ITEM('')
SURFACE()
);
#18=(
BOUNDED_SURFACE()
B_SPLINE_SURFACE(5,1,((#27292,#27293),(#27294,#27295),(#27296,#27297),(#27298,
#27299),(#27300,#27301),(#27302,#27303),(#27304,#27305),(#27306,#27307),
(#27308,#27309),(#27310,#27311),(#27312,#27313),(#27314,#27315),(#27316,
#27317),(#27318,#27319),(#27320,#27321),(#27322,#27323),(#27324,#27325),
(#27326,#27327),(#27328,#27329),(#27330,#27331),(#27332,#27333),(#27334,
#27335),(#27336,#27337),(#27338,#27339),(#27340,#27341),(#27342,#27343),
(#27344,#27345),(#27346,#27347),(#27348,#27349),(#27350,#27351),(#27352,
#27353),(#27354,#27355),(#27356,#27357),(#27358,#27359),(#27360,#27361),
(#27362,#27363),(#27364,#27365),(#27366,#27367),(#27368,#27369),(#27370,
#27371),(#27372,#27373),(#27374,#27375),(#27376,#27377),(#27378,#27379),
(#27380,#27381),(#27382,#27383),(#27384,#27385),(#27386,#27387),(#27388,
#27389),(#27390,#27391),(#27392,#27393),(#27394,#27395),(#27396,#27397),
(#27398,#27399),(#27400,#27401),(#27402,#27403),(#27404,#27405),(#27406,
#27407),(#27408,#27409),(#27410,#27411),(#27412,#27413),(#27414,#27415),
(#27416,#27417),(#27418,#27419),(#27420,#27421),(#27422,#27423),(#27424,
#27425),(#27426,#27427),(#27428,#27429),(#27430,#27431)),.UNSPECIFIED.,
 .F.,.F.,.F.)
B_SPLINE_SURFACE_WITH_KNOTS((6,1,1,1,1,1,1,1,1,1,1,1,1,1,1,1,1,1,1,1,1,
1,1,1,1,1,1,1,1,1,1,1,1,1,1,1,1,1,1,1,1,1,1,1,1,1,1,1,1,1,1,1,1,1,1,1,1,
1,1,1,1,1,1,1,1,6),(2,2),(-1.,-0.984615384615383,-0.969230769230768,-0.953846153846152,
-0.938461538461537,-0.923076923076922,-0.907692307692306,-0.892307692307691,
-0.876923076923076,-0.86153846153846,-0.846153846153845,-0.83076923076923,
-0.815384615384614,-0.799999999999999,-0.784615384615384,-0.769230769230768,
-0.753846153846153,-0.738461538461538,-0.723076923076922,-0.707692307692307,
-0.692307692307692,-0.676923076923076,-0.661538461538461,-0.646153846153846,
-0.63076923076923,-0.615384615384615,-0.6,-0.584615384615384,-0.569230769230769,
-0.553846153846154,-0.538461538461538,-0.523076923076923,-0.507692307692308,
-0.492307692307692,-0.476923076923077,-0.461538461538462,-0.446153846153846,
-0.430769230769231,-0.415384615384615,-0.4,-0.384615384615385,-0.369230769230769,
-0.353846153846154,-0.338461538461538,-0.323076923076923,-0.307692307692308,
-0.292307692307692,-0.276923076923077,-0.261538461538462,-0.246153846153846,
-0.230769230769231,-0.215384615384615,-0.2,-0.184615384615385,-0.169230769230769,
-0.153846153846154,-0.138461538461538,-0.123076923076923,-0.107692307692308,
-0.0923076923076923,-0.0769230769230769,-0.0615384615384615,-0.0461538461538462,
-0.0307692307692308,-0.0153846153846154,0.),(-1.,1.),.UNSPECIFIED.)
GEOMETRIC_REPRESENTATION_ITEM()
RATIONAL_B_SPLINE_SURFACE(((1.,1.),(1.,1.),(1.,1.),(1.,1.),(1.,1.),(1.,
1.),(1.,1.),(1.,1.),(1.,1.),(1.,1.),(1.,1.),(1.,1.),(1.,1.),(1.,1.),(1.,
1.),(1.,1.),(1.,1.),(1.,1.),(1.,1.),(1.,1.),(1.,1.),(1.,1.),(1.,1.),(1.,
1.),(1.,1.),(1.,1.),(1.,1.),(1.,1.),(1.,1.),(1.,1.),(1.,1.),(1.,1.),(1.,
1.),(1.,1.),(1.,1.),(1.,1.),(1.,1.),(1.,1.),(1.,1.),(1.,1.),(1.,1.),(1.,
1.),(1.,1.),(1.,1.),(1.,1.),(1.,1.),(1.,1.),(1.,1.),(1.,1.),(1.,1.),(1.,
1.),(1.,1.),(1.,1.),(1.,1.),(1.,1.),(1.,1.),(1.,1.),(1.,1.),(1.,1.),(1.,
1.),(1.,1.),(1.,1.),(1.,1.),(1.,1.),(1.,1.),(1.,1.),(1.,1.),(1.,1.),(1.,
1.),(1.,1.)))
REPRESENTATION_ITEM('')
SURFACE()
);
#19=(
BOUNDED_SURFACE()
B_SPLINE_SURFACE(5,1,((#27508,#27509),(#27510,#27511),(#27512,#27513),(#27514,
#27515),(#27516,#27517),(#27518,#27519),(#27520,#27521),(#27522,#27523),
(#27524,#27525),(#27526,#27527),(#27528,#27529),(#27530,#27531),(#27532,
#27533),(#27534,#27535),(#27536,#27537),(#27538,#27539),(#27540,#27541),
(#27542,#27543),(#27544,#27545),(#27546,#27547),(#27548,#27549),(#27550,
#27551),(#27552,#27553),(#27554,#27555),(#27556,#27557),(#27558,#27559),
(#27560,#27561),(#27562,#27563),(#27564,#27565),(#27566,#27567),(#27568,
#27569),(#27570,#27571),(#27572,#27573),(#27574,#27575),(#27576,#27577),
(#27578,#27579),(#27580,#27581),(#27582,#27583),(#27584,#27585),(#27586,
#27587),(#27588,#27589),(#27590,#27591),(#27592,#27593),(#27594,#27595),
(#27596,#27597),(#27598,#27599),(#27600,#27601),(#27602,#27603),(#27604,
#27605),(#27606,#27607),(#27608,#27609),(#27610,#27611),(#27612,#27613),
(#27614,#27615),(#27616,#27617),(#27618,#27619),(#27620,#27621),(#27622,
#27623),(#27624,#27625),(#27626,#27627),(#27628,#27629),(#27630,#27631),
(#27632,#27633),(#27634,#27635),(#27636,#27637),(#27638,#27639),(#27640,
#27641),(#27642,#27643),(#27644,#27645),(#27646,#27647)),.UNSPECIFIED.,
 .F.,.F.,.F.)
B_SPLINE_SURFACE_WITH_KNOTS((6,1,1,1,1,1,1,1,1,1,1,1,1,1,1,1,1,1,1,1,1,
1,1,1,1,1,1,1,1,1,1,1,1,1,1,1,1,1,1,1,1,1,1,1,1,1,1,1,1,1,1,1,1,1,1,1,1,
1,1,1,1,1,1,1,1,6),(2,2),(-1.,-0.984615384615383,-0.969230769230768,-0.953846153846152,
-0.938461538461537,-0.923076923076922,-0.907692307692306,-0.892307692307691,
-0.876923076923076,-0.86153846153846,-0.846153846153845,-0.83076923076923,
-0.815384615384614,-0.799999999999999,-0.784615384615384,-0.769230769230768,
-0.753846153846153,-0.738461538461538,-0.723076923076922,-0.707692307692307,
-0.692307692307692,-0.676923076923076,-0.661538461538461,-0.646153846153846,
-0.63076923076923,-0.615384615384615,-0.6,-0.584615384615384,-0.569230769230769,
-0.553846153846154,-0.538461538461538,-0.523076923076923,-0.507692307692308,
-0.492307692307692,-0.476923076923077,-0.461538461538462,-0.446153846153846,
-0.430769230769231,-0.415384615384615,-0.4,-0.384615384615385,-0.369230769230769,
-0.353846153846154,-0.338461538461538,-0.323076923076923,-0.307692307692308,
-0.292307692307692,-0.276923076923077,-0.261538461538462,-0.246153846153846,
-0.230769230769231,-0.215384615384615,-0.2,-0.184615384615385,-0.169230769230769,
-0.153846153846154,-0.138461538461538,-0.123076923076923,-0.107692307692308,
-0.0923076923076923,-0.0769230769230769,-0.0615384615384615,-0.0461538461538462,
-0.0307692307692308,-0.0153846153846154,0.),(-1.,1.),.UNSPECIFIED.)
GEOMETRIC_REPRESENTATION_ITEM()
RATIONAL_B_SPLINE_SURFACE(((1.,1.),(1.,1.),(1.,1.),(1.,1.),(1.,1.),(1.,
1.),(1.,1.),(1.,1.),(1.,1.),(1.,1.),(1.,1.),(1.,1.),(1.,1.),(1.,1.),(1.,
1.),(1.,1.),(1.,1.),(1.,1.),(1.,1.),(1.,1.),(1.,1.),(1.,1.),(1.,1.),(1.,
1.),(1.,1.),(1.,1.),(1.,1.),(1.,1.),(1.,1.),(1.,1.),(1.,1.),(1.,1.),(1.,
1.),(1.,1.),(1.,1.),(1.,1.),(1.,1.),(1.,1.),(1.,1.),(1.,1.),(1.,1.),(1.,
1.),(1.,1.),(1.,1.),(1.,1.),(1.,1.),(1.,1.),(1.,1.),(1.,1.),(1.,1.),(1.,
1.),(1.,1.),(1.,1.),(1.,1.),(1.,1.),(1.,1.),(1.,1.),(1.,1.),(1.,1.),(1.,
1.),(1.,1.),(1.,1.),(1.,1.),(1.,1.),(1.,1.),(1.,1.),(1.,1.),(1.,1.),(1.,
1.),(1.,1.)))
REPRESENTATION_ITEM('')
SURFACE()
);
#20=(
BOUNDED_SURFACE()
B_SPLINE_SURFACE(5,1,((#27724,#27725),(#27726,#27727),(#27728,#27729),(#27730,
#27731),(#27732,#27733),(#27734,#27735),(#27736,#27737),(#27738,#27739),
(#27740,#27741),(#27742,#27743),(#27744,#27745),(#27746,#27747),(#27748,
#27749),(#27750,#27751),(#27752,#27753),(#27754,#27755),(#27756,#27757),
(#27758,#27759),(#27760,#27761),(#27762,#27763),(#27764,#27765),(#27766,
#27767),(#27768,#27769),(#27770,#27771),(#27772,#27773),(#27774,#27775),
(#27776,#27777),(#27778,#27779),(#27780,#27781),(#27782,#27783),(#27784,
#27785),(#27786,#27787),(#27788,#27789),(#27790,#27791),(#27792,#27793),
(#27794,#27795),(#27796,#27797),(#27798,#27799),(#27800,#27801),(#27802,
#27803),(#27804,#27805),(#27806,#27807),(#27808,#27809),(#27810,#27811),
(#27812,#27813),(#27814,#27815),(#27816,#27817),(#27818,#27819),(#27820,
#27821),(#27822,#27823),(#27824,#27825),(#27826,#27827),(#27828,#27829),
(#27830,#27831),(#27832,#27833),(#27834,#27835),(#27836,#27837),(#27838,
#27839),(#27840,#27841),(#27842,#27843),(#27844,#27845),(#27846,#27847),
(#27848,#27849),(#27850,#27851),(#27852,#27853),(#27854,#27855),(#27856,
#27857),(#27858,#27859),(#27860,#27861),(#27862,#27863)),.UNSPECIFIED.,
 .F.,.F.,.F.)
B_SPLINE_SURFACE_WITH_KNOTS((6,1,1,1,1,1,1,1,1,1,1,1,1,1,1,1,1,1,1,1,1,
1,1,1,1,1,1,1,1,1,1,1,1,1,1,1,1,1,1,1,1,1,1,1,1,1,1,1,1,1,1,1,1,1,1,1,1,
1,1,1,1,1,1,1,1,6),(2,2),(-1.,-0.984615384615383,-0.969230769230768,-0.953846153846152,
-0.938461538461537,-0.923076923076922,-0.907692307692306,-0.892307692307691,
-0.876923076923076,-0.86153846153846,-0.846153846153845,-0.83076923076923,
-0.815384615384614,-0.799999999999999,-0.784615384615384,-0.769230769230768,
-0.753846153846153,-0.738461538461538,-0.723076923076922,-0.707692307692307,
-0.692307692307692,-0.676923076923076,-0.661538461538461,-0.646153846153846,
-0.63076923076923,-0.615384615384615,-0.6,-0.584615384615384,-0.569230769230769,
-0.553846153846154,-0.538461538461538,-0.523076923076923,-0.507692307692308,
-0.492307692307692,-0.476923076923077,-0.461538461538462,-0.446153846153846,
-0.430769230769231,-0.415384615384615,-0.4,-0.384615384615385,-0.369230769230769,
-0.353846153846154,-0.338461538461538,-0.323076923076923,-0.307692307692308,
-0.292307692307692,-0.276923076923077,-0.261538461538462,-0.246153846153846,
-0.230769230769231,-0.215384615384615,-0.2,-0.184615384615385,-0.169230769230769,
-0.153846153846154,-0.138461538461538,-0.123076923076923,-0.107692307692308,
-0.0923076923076923,-0.0769230769230769,-0.0615384615384615,-0.0461538461538462,
-0.0307692307692308,-0.0153846153846154,0.),(-1.,1.),.UNSPECIFIED.)
GEOMETRIC_REPRESENTATION_ITEM()
RATIONAL_B_SPLINE_SURFACE(((1.,1.),(1.,1.),(1.,1.),(1.,1.),(1.,1.),(1.,
1.),(1.,1.),(1.,1.),(1.,1.),(1.,1.),(1.,1.),(1.,1.),(1.,1.),(1.,1.),(1.,
1.),(1.,1.),(1.,1.),(1.,1.),(1.,1.),(1.,1.),(1.,1.),(1.,1.),(1.,1.),(1.,
1.),(1.,1.),(1.,1.),(1.,1.),(1.,1.),(1.,1.),(1.,1.),(1.,1.),(1.,1.),(1.,
1.),(1.,1.),(1.,1.),(1.,1.),(1.,1.),(1.,1.),(1.,1.),(1.,1.),(1.,1.),(1.,
1.),(1.,1.),(1.,1.),(1.,1.),(1.,1.),(1.,1.),(1.,1.),(1.,1.),(1.,1.),(1.,
1.),(1.,1.),(1.,1.),(1.,1.),(1.,1.),(1.,1.),(1.,1.),(1.,1.),(1.,1.),(1.,
1.),(1.,1.),(1.,1.),(1.,1.),(1.,1.),(1.,1.),(1.,1.),(1.,1.),(1.,1.),(1.,
1.),(1.,1.)))
REPRESENTATION_ITEM('')
SURFACE()
);
#21=(
BOUNDED_SURFACE()
B_SPLINE_SURFACE(5,1,((#27940,#27941),(#27942,#27943),(#27944,#27945),(#27946,
#27947),(#27948,#27949),(#27950,#27951),(#27952,#27953),(#27954,#27955),
(#27956,#27957),(#27958,#27959),(#27960,#27961),(#27962,#27963),(#27964,
#27965),(#27966,#27967),(#27968,#27969),(#27970,#27971),(#27972,#27973),
(#27974,#27975),(#27976,#27977),(#27978,#27979),(#27980,#27981),(#27982,
#27983),(#27984,#27985),(#27986,#27987),(#27988,#27989),(#27990,#27991),
(#27992,#27993),(#27994,#27995),(#27996,#27997),(#27998,#27999),(#28000,
#28001),(#28002,#28003),(#28004,#28005),(#28006,#28007),(#28008,#28009),
(#28010,#28011),(#28012,#28013),(#28014,#28015),(#28016,#28017),(#28018,
#28019),(#28020,#28021),(#28022,#28023),(#28024,#28025),(#28026,#28027),
(#28028,#28029),(#28030,#28031),(#28032,#28033),(#28034,#28035),(#28036,
#28037),(#28038,#28039),(#28040,#28041),(#28042,#28043),(#28044,#28045),
(#28046,#28047),(#28048,#28049),(#28050,#28051),(#28052,#28053),(#28054,
#28055),(#28056,#28057),(#28058,#28059),(#28060,#28061),(#28062,#28063),
(#28064,#28065),(#28066,#28067),(#28068,#28069),(#28070,#28071),(#28072,
#28073),(#28074,#28075),(#28076,#28077),(#28078,#28079)),.UNSPECIFIED.,
 .F.,.F.,.F.)
B_SPLINE_SURFACE_WITH_KNOTS((6,1,1,1,1,1,1,1,1,1,1,1,1,1,1,1,1,1,1,1,1,
1,1,1,1,1,1,1,1,1,1,1,1,1,1,1,1,1,1,1,1,1,1,1,1,1,1,1,1,1,1,1,1,1,1,1,1,
1,1,1,1,1,1,1,1,6),(2,2),(-1.,-0.984615384615383,-0.969230769230768,-0.953846153846152,
-0.938461538461537,-0.923076923076922,-0.907692307692306,-0.892307692307691,
-0.876923076923076,-0.86153846153846,-0.846153846153845,-0.83076923076923,
-0.815384615384614,-0.799999999999999,-0.784615384615384,-0.769230769230768,
-0.753846153846153,-0.738461538461538,-0.723076923076922,-0.707692307692307,
-0.692307692307692,-0.676923076923076,-0.661538461538461,-0.646153846153846,
-0.63076923076923,-0.615384615384615,-0.6,-0.584615384615384,-0.569230769230769,
-0.553846153846154,-0.538461538461538,-0.523076923076923,-0.507692307692308,
-0.492307692307692,-0.476923076923077,-0.461538461538462,-0.446153846153846,
-0.430769230769231,-0.415384615384615,-0.4,-0.384615384615385,-0.369230769230769,
-0.353846153846154,-0.338461538461538,-0.323076923076923,-0.307692307692308,
-0.292307692307692,-0.276923076923077,-0.261538461538462,-0.246153846153846,
-0.230769230769231,-0.215384615384615,-0.2,-0.184615384615385,-0.169230769230769,
-0.153846153846154,-0.138461538461538,-0.123076923076923,-0.107692307692308,
-0.0923076923076923,-0.0769230769230769,-0.0615384615384615,-0.0461538461538462,
-0.0307692307692308,-0.0153846153846154,0.),(-1.,1.),.UNSPECIFIED.)
GEOMETRIC_REPRESENTATION_ITEM()
RATIONAL_B_SPLINE_SURFACE(((1.,1.),(1.,1.),(1.,1.),(1.,1.),(1.,1.),(1.,
1.),(1.,1.),(1.,1.),(1.,1.),(1.,1.),(1.,1.),(1.,1.),(1.,1.),(1.,1.),(1.,
1.),(1.,1.),(1.,1.),(1.,1.),(1.,1.),(1.,1.),(1.,1.),(1.,1.),(1.,1.),(1.,
1.),(1.,1.),(1.,1.),(1.,1.),(1.,1.),(1.,1.),(1.,1.),(1.,1.),(1.,1.),(1.,
1.),(1.,1.),(1.,1.),(1.,1.),(1.,1.),(1.,1.),(1.,1.),(1.,1.),(1.,1.),(1.,
1.),(1.,1.),(1.,1.),(1.,1.),(1.,1.),(1.,1.),(1.,1.),(1.,1.),(1.,1.),(1.,
1.),(1.,1.),(1.,1.),(1.,1.),(1.,1.),(1.,1.),(1.,1.),(1.,1.),(1.,1.),(1.,
1.),(1.,1.),(1.,1.),(1.,1.),(1.,1.),(1.,1.),(1.,1.),(1.,1.),(1.,1.),(1.,
1.),(1.,1.)))
REPRESENTATION_ITEM('')
SURFACE()
);
#22=(
BOUNDED_SURFACE()
B_SPLINE_SURFACE(5,1,((#28156,#28157),(#28158,#28159),(#28160,#28161),(#28162,
#28163),(#28164,#28165),(#28166,#28167),(#28168,#28169),(#28170,#28171),
(#28172,#28173),(#28174,#28175),(#28176,#28177),(#28178,#28179),(#28180,
#28181),(#28182,#28183),(#28184,#28185),(#28186,#28187),(#28188,#28189),
(#28190,#28191),(#28192,#28193),(#28194,#28195),(#28196,#28197),(#28198,
#28199),(#28200,#28201),(#28202,#28203),(#28204,#28205),(#28206,#28207),
(#28208,#28209),(#28210,#28211),(#28212,#28213),(#28214,#28215),(#28216,
#28217),(#28218,#28219),(#28220,#28221),(#28222,#28223),(#28224,#28225),
(#28226,#28227),(#28228,#28229),(#28230,#28231),(#28232,#28233),(#28234,
#28235),(#28236,#28237),(#28238,#28239),(#28240,#28241),(#28242,#28243),
(#28244,#28245),(#28246,#28247),(#28248,#28249),(#28250,#28251),(#28252,
#28253),(#28254,#28255),(#28256,#28257),(#28258,#28259),(#28260,#28261),
(#28262,#28263),(#28264,#28265),(#28266,#28267),(#28268,#28269),(#28270,
#28271),(#28272,#28273),(#28274,#28275),(#28276,#28277),(#28278,#28279),
(#28280,#28281),(#28282,#28283),(#28284,#28285),(#28286,#28287),(#28288,
#28289),(#28290,#28291),(#28292,#28293),(#28294,#28295)),.UNSPECIFIED.,
 .F.,.F.,.F.)
B_SPLINE_SURFACE_WITH_KNOTS((6,1,1,1,1,1,1,1,1,1,1,1,1,1,1,1,1,1,1,1,1,
1,1,1,1,1,1,1,1,1,1,1,1,1,1,1,1,1,1,1,1,1,1,1,1,1,1,1,1,1,1,1,1,1,1,1,1,
1,1,1,1,1,1,1,1,6),(2,2),(-1.,-0.984615384615383,-0.969230769230768,-0.953846153846152,
-0.938461538461537,-0.923076923076922,-0.907692307692306,-0.892307692307691,
-0.876923076923076,-0.86153846153846,-0.846153846153845,-0.83076923076923,
-0.815384615384614,-0.799999999999999,-0.784615384615384,-0.769230769230768,
-0.753846153846153,-0.738461538461538,-0.723076923076922,-0.707692307692307,
-0.692307692307692,-0.676923076923076,-0.661538461538461,-0.646153846153846,
-0.63076923076923,-0.615384615384615,-0.6,-0.584615384615384,-0.569230769230769,
-0.553846153846154,-0.538461538461538,-0.523076923076923,-0.507692307692308,
-0.492307692307692,-0.476923076923077,-0.461538461538462,-0.446153846153846,
-0.430769230769231,-0.415384615384615,-0.4,-0.384615384615385,-0.369230769230769,
-0.353846153846154,-0.338461538461538,-0.323076923076923,-0.307692307692308,
-0.292307692307692,-0.276923076923077,-0.261538461538462,-0.246153846153846,
-0.230769230769231,-0.215384615384615,-0.2,-0.184615384615385,-0.169230769230769,
-0.153846153846154,-0.138461538461538,-0.123076923076923,-0.107692307692308,
-0.0923076923076923,-0.0769230769230769,-0.0615384615384615,-0.0461538461538462,
-0.0307692307692308,-0.0153846153846154,0.),(-1.,1.),.UNSPECIFIED.)
GEOMETRIC_REPRESENTATION_ITEM()
RATIONAL_B_SPLINE_SURFACE(((1.,1.),(1.,1.),(1.,1.),(1.,1.),(1.,1.),(1.,
1.),(1.,1.),(1.,1.),(1.,1.),(1.,1.),(1.,1.),(1.,1.),(1.,1.),(1.,1.),(1.,
1.),(1.,1.),(1.,1.),(1.,1.),(1.,1.),(1.,1.),(1.,1.),(1.,1.),(1.,1.),(1.,
1.),(1.,1.),(1.,1.),(1.,1.),(1.,1.),(1.,1.),(1.,1.),(1.,1.),(1.,1.),(1.,
1.),(1.,1.),(1.,1.),(1.,1.),(1.,1.),(1.,1.),(1.,1.),(1.,1.),(1.,1.),(1.,
1.),(1.,1.),(1.,1.),(1.,1.),(1.,1.),(1.,1.),(1.,1.),(1.,1.),(1.,1.),(1.,
1.),(1.,1.),(1.,1.),(1.,1.),(1.,1.),(1.,1.),(1.,1.),(1.,1.),(1.,1.),(1.,
1.),(1.,1.),(1.,1.),(1.,1.),(1.,1.),(1.,1.),(1.,1.),(1.,1.),(1.,1.),(1.,
1.),(1.,1.)))
REPRESENTATION_ITEM('')
SURFACE()
);
#23=(
BOUNDED_SURFACE()
B_SPLINE_SURFACE(5,1,((#28372,#28373),(#28374,#28375),(#28376,#28377),(#28378,
#28379),(#28380,#28381),(#28382,#28383),(#28384,#28385),(#28386,#28387),
(#28388,#28389),(#28390,#28391),(#28392,#28393),(#28394,#28395),(#28396,
#28397),(#28398,#28399),(#28400,#28401),(#28402,#28403),(#28404,#28405),
(#28406,#28407),(#28408,#28409),(#28410,#28411),(#28412,#28413),(#28414,
#28415),(#28416,#28417),(#28418,#28419),(#28420,#28421),(#28422,#28423),
(#28424,#28425),(#28426,#28427),(#28428,#28429),(#28430,#28431),(#28432,
#28433),(#28434,#28435),(#28436,#28437),(#28438,#28439),(#28440,#28441),
(#28442,#28443),(#28444,#28445),(#28446,#28447),(#28448,#28449),(#28450,
#28451),(#28452,#28453),(#28454,#28455),(#28456,#28457),(#28458,#28459),
(#28460,#28461),(#28462,#28463),(#28464,#28465),(#28466,#28467),(#28468,
#28469),(#28470,#28471),(#28472,#28473),(#28474,#28475),(#28476,#28477),
(#28478,#28479),(#28480,#28481),(#28482,#28483),(#28484,#28485),(#28486,
#28487),(#28488,#28489),(#28490,#28491),(#28492,#28493),(#28494,#28495),
(#28496,#28497),(#28498,#28499),(#28500,#28501),(#28502,#28503),(#28504,
#28505),(#28506,#28507),(#28508,#28509),(#28510,#28511)),.UNSPECIFIED.,
 .F.,.F.,.F.)
B_SPLINE_SURFACE_WITH_KNOTS((6,1,1,1,1,1,1,1,1,1,1,1,1,1,1,1,1,1,1,1,1,
1,1,1,1,1,1,1,1,1,1,1,1,1,1,1,1,1,1,1,1,1,1,1,1,1,1,1,1,1,1,1,1,1,1,1,1,
1,1,1,1,1,1,1,1,6),(2,2),(-1.,-0.984615384615383,-0.969230769230768,-0.953846153846152,
-0.938461538461537,-0.923076923076922,-0.907692307692306,-0.892307692307691,
-0.876923076923076,-0.86153846153846,-0.846153846153845,-0.83076923076923,
-0.815384615384614,-0.799999999999999,-0.784615384615384,-0.769230769230768,
-0.753846153846153,-0.738461538461538,-0.723076923076922,-0.707692307692307,
-0.692307692307692,-0.676923076923076,-0.661538461538461,-0.646153846153846,
-0.63076923076923,-0.615384615384615,-0.6,-0.584615384615384,-0.569230769230769,
-0.553846153846154,-0.538461538461538,-0.523076923076923,-0.507692307692308,
-0.492307692307692,-0.476923076923077,-0.461538461538462,-0.446153846153846,
-0.430769230769231,-0.415384615384615,-0.4,-0.384615384615385,-0.369230769230769,
-0.353846153846154,-0.338461538461538,-0.323076923076923,-0.307692307692308,
-0.292307692307692,-0.276923076923077,-0.261538461538462,-0.246153846153846,
-0.230769230769231,-0.215384615384615,-0.2,-0.184615384615385,-0.169230769230769,
-0.153846153846154,-0.138461538461538,-0.123076923076923,-0.107692307692308,
-0.0923076923076923,-0.0769230769230769,-0.0615384615384615,-0.0461538461538462,
-0.0307692307692308,-0.0153846153846154,0.),(-1.,1.),.UNSPECIFIED.)
GEOMETRIC_REPRESENTATION_ITEM()
RATIONAL_B_SPLINE_SURFACE(((1.,1.),(1.,1.),(1.,1.),(1.,1.),(1.,1.),(1.,
1.),(1.,1.),(1.,1.),(1.,1.),(1.,1.),(1.,1.),(1.,1.),(1.,1.),(1.,1.),(1.,
1.),(1.,1.),(1.,1.),(1.,1.),(1.,1.),(1.,1.),(1.,1.),(1.,1.),(1.,1.),(1.,
1.),(1.,1.),(1.,1.),(1.,1.),(1.,1.),(1.,1.),(1.,1.),(1.,1.),(1.,1.),(1.,
1.),(1.,1.),(1.,1.),(1.,1.),(1.,1.),(1.,1.),(1.,1.),(1.,1.),(1.,1.),(1.,
1.),(1.,1.),(1.,1.),(1.,1.),(1.,1.),(1.,1.),(1.,1.),(1.,1.),(1.,1.),(1.,
1.),(1.,1.),(1.,1.),(1.,1.),(1.,1.),(1.,1.),(1.,1.),(1.,1.),(1.,1.),(1.,
1.),(1.,1.),(1.,1.),(1.,1.),(1.,1.),(1.,1.),(1.,1.),(1.,1.),(1.,1.),(1.,
1.),(1.,1.)))
REPRESENTATION_ITEM('')
SURFACE()
);
#24=(
BOUNDED_SURFACE()
B_SPLINE_SURFACE(5,1,((#28588,#28589),(#28590,#28591),(#28592,#28593),(#28594,
#28595),(#28596,#28597),(#28598,#28599),(#28600,#28601),(#28602,#28603),
(#28604,#28605),(#28606,#28607),(#28608,#28609),(#28610,#28611),(#28612,
#28613),(#28614,#28615),(#28616,#28617),(#28618,#28619),(#28620,#28621),
(#28622,#28623),(#28624,#28625),(#28626,#28627),(#28628,#28629),(#28630,
#28631),(#28632,#28633),(#28634,#28635),(#28636,#28637),(#28638,#28639),
(#28640,#28641),(#28642,#28643),(#28644,#28645),(#28646,#28647),(#28648,
#28649),(#28650,#28651),(#28652,#28653),(#28654,#28655),(#28656,#28657),
(#28658,#28659),(#28660,#28661),(#28662,#28663),(#28664,#28665),(#28666,
#28667),(#28668,#28669),(#28670,#28671),(#28672,#28673),(#28674,#28675),
(#28676,#28677),(#28678,#28679),(#28680,#28681),(#28682,#28683),(#28684,
#28685),(#28686,#28687),(#28688,#28689),(#28690,#28691),(#28692,#28693),
(#28694,#28695),(#28696,#28697),(#28698,#28699),(#28700,#28701),(#28702,
#28703),(#28704,#28705),(#28706,#28707),(#28708,#28709),(#28710,#28711),
(#28712,#28713),(#28714,#28715),(#28716,#28717),(#28718,#28719),(#28720,
#28721),(#28722,#28723),(#28724,#28725),(#28726,#28727)),.UNSPECIFIED.,
 .F.,.F.,.F.)
B_SPLINE_SURFACE_WITH_KNOTS((6,1,1,1,1,1,1,1,1,1,1,1,1,1,1,1,1,1,1,1,1,
1,1,1,1,1,1,1,1,1,1,1,1,1,1,1,1,1,1,1,1,1,1,1,1,1,1,1,1,1,1,1,1,1,1,1,1,
1,1,1,1,1,1,1,1,6),(2,2),(-1.,-0.984615384615383,-0.969230769230768,-0.953846153846152,
-0.938461538461537,-0.923076923076922,-0.907692307692306,-0.892307692307691,
-0.876923076923076,-0.86153846153846,-0.846153846153845,-0.83076923076923,
-0.815384615384614,-0.799999999999999,-0.784615384615384,-0.769230769230768,
-0.753846153846153,-0.738461538461538,-0.723076923076922,-0.707692307692307,
-0.692307692307692,-0.676923076923076,-0.661538461538461,-0.646153846153846,
-0.63076923076923,-0.615384615384615,-0.6,-0.584615384615384,-0.569230769230769,
-0.553846153846154,-0.538461538461538,-0.523076923076923,-0.507692307692308,
-0.492307692307692,-0.476923076923077,-0.461538461538462,-0.446153846153846,
-0.430769230769231,-0.415384615384615,-0.4,-0.384615384615385,-0.369230769230769,
-0.353846153846154,-0.338461538461538,-0.323076923076923,-0.307692307692308,
-0.292307692307692,-0.276923076923077,-0.261538461538462,-0.246153846153846,
-0.230769230769231,-0.215384615384615,-0.2,-0.184615384615385,-0.169230769230769,
-0.153846153846154,-0.138461538461538,-0.123076923076923,-0.107692307692308,
-0.0923076923076923,-0.0769230769230769,-0.0615384615384615,-0.0461538461538462,
-0.0307692307692308,-0.0153846153846154,0.),(-1.,1.),.UNSPECIFIED.)
GEOMETRIC_REPRESENTATION_ITEM()
RATIONAL_B_SPLINE_SURFACE(((1.,1.),(1.,1.),(1.,1.),(1.,1.),(1.,1.),(1.,
1.),(1.,1.),(1.,1.),(1.,1.),(1.,1.),(1.,1.),(1.,1.),(1.,1.),(1.,1.),(1.,
1.),(1.,1.),(1.,1.),(1.,1.),(1.,1.),(1.,1.),(1.,1.),(1.,1.),(1.,1.),(1.,
1.),(1.,1.),(1.,1.),(1.,1.),(1.,1.),(1.,1.),(1.,1.),(1.,1.),(1.,1.),(1.,
1.),(1.,1.),(1.,1.),(1.,1.),(1.,1.),(1.,1.),(1.,1.),(1.,1.),(1.,1.),(1.,
1.),(1.,1.),(1.,1.),(1.,1.),(1.,1.),(1.,1.),(1.,1.),(1.,1.),(1.,1.),(1.,
1.),(1.,1.),(1.,1.),(1.,1.),(1.,1.),(1.,1.),(1.,1.),(1.,1.),(1.,1.),(1.,
1.),(1.,1.),(1.,1.),(1.,1.),(1.,1.),(1.,1.),(1.,1.),(1.,1.),(1.,1.),(1.,
1.),(1.,1.)))
REPRESENTATION_ITEM('')
SURFACE()
);
#25=(
BOUNDED_SURFACE()
B_SPLINE_SURFACE(5,1,((#28804,#28805),(#28806,#28807),(#28808,#28809),(#28810,
#28811),(#28812,#28813),(#28814,#28815),(#28816,#28817),(#28818,#28819),
(#28820,#28821),(#28822,#28823),(#28824,#28825),(#28826,#28827),(#28828,
#28829),(#28830,#28831),(#28832,#28833),(#28834,#28835),(#28836,#28837),
(#28838,#28839),(#28840,#28841),(#28842,#28843),(#28844,#28845),(#28846,
#28847),(#28848,#28849),(#28850,#28851),(#28852,#28853),(#28854,#28855),
(#28856,#28857),(#28858,#28859),(#28860,#28861),(#28862,#28863),(#28864,
#28865),(#28866,#28867),(#28868,#28869),(#28870,#28871),(#28872,#28873),
(#28874,#28875),(#28876,#28877),(#28878,#28879),(#28880,#28881),(#28882,
#28883),(#28884,#28885),(#28886,#28887),(#28888,#28889),(#28890,#28891),
(#28892,#28893),(#28894,#28895),(#28896,#28897),(#28898,#28899),(#28900,
#28901),(#28902,#28903),(#28904,#28905),(#28906,#28907),(#28908,#28909),
(#28910,#28911),(#28912,#28913),(#28914,#28915),(#28916,#28917),(#28918,
#28919),(#28920,#28921),(#28922,#28923),(#28924,#28925),(#28926,#28927),
(#28928,#28929),(#28930,#28931),(#28932,#28933),(#28934,#28935),(#28936,
#28937),(#28938,#28939),(#28940,#28941),(#28942,#28943)),.UNSPECIFIED.,
 .F.,.F.,.F.)
B_SPLINE_SURFACE_WITH_KNOTS((6,1,1,1,1,1,1,1,1,1,1,1,1,1,1,1,1,1,1,1,1,
1,1,1,1,1,1,1,1,1,1,1,1,1,1,1,1,1,1,1,1,1,1,1,1,1,1,1,1,1,1,1,1,1,1,1,1,
1,1,1,1,1,1,1,1,6),(2,2),(-1.,-0.984615384615383,-0.969230769230768,-0.953846153846152,
-0.938461538461537,-0.923076923076922,-0.907692307692306,-0.892307692307691,
-0.876923076923076,-0.86153846153846,-0.846153846153845,-0.83076923076923,
-0.815384615384614,-0.799999999999999,-0.784615384615384,-0.769230769230768,
-0.753846153846153,-0.738461538461538,-0.723076923076922,-0.707692307692307,
-0.692307692307692,-0.676923076923076,-0.661538461538461,-0.646153846153846,
-0.63076923076923,-0.615384615384615,-0.6,-0.584615384615384,-0.569230769230769,
-0.553846153846154,-0.538461538461538,-0.523076923076923,-0.507692307692308,
-0.492307692307692,-0.476923076923077,-0.461538461538462,-0.446153846153846,
-0.430769230769231,-0.415384615384615,-0.4,-0.384615384615385,-0.369230769230769,
-0.353846153846154,-0.338461538461538,-0.323076923076923,-0.307692307692308,
-0.292307692307692,-0.276923076923077,-0.261538461538462,-0.246153846153846,
-0.230769230769231,-0.215384615384615,-0.2,-0.184615384615385,-0.169230769230769,
-0.153846153846154,-0.138461538461538,-0.123076923076923,-0.107692307692308,
-0.0923076923076923,-0.0769230769230769,-0.0615384615384615,-0.0461538461538462,
-0.0307692307692308,-0.0153846153846154,0.),(-1.,1.),.UNSPECIFIED.)
GEOMETRIC_REPRESENTATION_ITEM()
RATIONAL_B_SPLINE_SURFACE(((1.,1.),(1.,1.),(1.,1.),(1.,1.),(1.,1.),(1.,
1.),(1.,1.),(1.,1.),(1.,1.),(1.,1.),(1.,1.),(1.,1.),(1.,1.),(1.,1.),(1.,
1.),(1.,1.),(1.,1.),(1.,1.),(1.,1.),(1.,1.),(1.,1.),(1.,1.),(1.,1.),(1.,
1.),(1.,1.),(1.,1.),(1.,1.),(1.,1.),(1.,1.),(1.,1.),(1.,1.),(1.,1.),(1.,
1.),(1.,1.),(1.,1.),(1.,1.),(1.,1.),(1.,1.),(1.,1.),(1.,1.),(1.,1.),(1.,
1.),(1.,1.),(1.,1.),(1.,1.),(1.,1.),(1.,1.),(1.,1.),(1.,1.),(1.,1.),(1.,
1.),(1.,1.),(1.,1.),(1.,1.),(1.,1.),(1.,1.),(1.,1.),(1.,1.),(1.,1.),(1.,
1.),(1.,1.),(1.,1.),(1.,1.),(1.,1.),(1.,1.),(1.,1.),(1.,1.),(1.,1.),(1.,
1.),(1.,1.)))
REPRESENTATION_ITEM('')
SURFACE()
);
#26=(
BOUNDED_SURFACE()
B_SPLINE_SURFACE(5,1,((#29020,#29021),(#29022,#29023),(#29024,#29025),(#29026,
#29027),(#29028,#29029),(#29030,#29031),(#29032,#29033),(#29034,#29035),
(#29036,#29037),(#29038,#29039),(#29040,#29041),(#29042,#29043),(#29044,
#29045),(#29046,#29047),(#29048,#29049),(#29050,#29051),(#29052,#29053),
(#29054,#29055),(#29056,#29057),(#29058,#29059),(#29060,#29061),(#29062,
#29063),(#29064,#29065),(#29066,#29067),(#29068,#29069),(#29070,#29071),
(#29072,#29073),(#29074,#29075),(#29076,#29077),(#29078,#29079),(#29080,
#29081),(#29082,#29083),(#29084,#29085),(#29086,#29087),(#29088,#29089),
(#29090,#29091),(#29092,#29093),(#29094,#29095),(#29096,#29097),(#29098,
#29099),(#29100,#29101),(#29102,#29103),(#29104,#29105),(#29106,#29107),
(#29108,#29109),(#29110,#29111),(#29112,#29113),(#29114,#29115),(#29116,
#29117),(#29118,#29119),(#29120,#29121),(#29122,#29123),(#29124,#29125),
(#29126,#29127),(#29128,#29129),(#29130,#29131),(#29132,#29133),(#29134,
#29135),(#29136,#29137),(#29138,#29139),(#29140,#29141),(#29142,#29143),
(#29144,#29145),(#29146,#29147),(#29148,#29149),(#29150,#29151),(#29152,
#29153),(#29154,#29155),(#29156,#29157),(#29158,#29159)),.UNSPECIFIED.,
 .F.,.F.,.F.)
B_SPLINE_SURFACE_WITH_KNOTS((6,1,1,1,1,1,1,1,1,1,1,1,1,1,1,1,1,1,1,1,1,
1,1,1,1,1,1,1,1,1,1,1,1,1,1,1,1,1,1,1,1,1,1,1,1,1,1,1,1,1,1,1,1,1,1,1,1,
1,1,1,1,1,1,1,1,6),(2,2),(-1.,-0.984615384615383,-0.969230769230768,-0.953846153846152,
-0.938461538461537,-0.923076923076922,-0.907692307692306,-0.892307692307691,
-0.876923076923076,-0.86153846153846,-0.846153846153845,-0.83076923076923,
-0.815384615384614,-0.799999999999999,-0.784615384615384,-0.769230769230768,
-0.753846153846153,-0.738461538461538,-0.723076923076922,-0.707692307692307,
-0.692307692307692,-0.676923076923076,-0.661538461538461,-0.646153846153846,
-0.63076923076923,-0.615384615384615,-0.6,-0.584615384615384,-0.569230769230769,
-0.553846153846154,-0.538461538461538,-0.523076923076923,-0.507692307692308,
-0.492307692307692,-0.476923076923077,-0.461538461538462,-0.446153846153846,
-0.430769230769231,-0.415384615384615,-0.4,-0.384615384615385,-0.369230769230769,
-0.353846153846154,-0.338461538461538,-0.323076923076923,-0.307692307692308,
-0.292307692307692,-0.276923076923077,-0.261538461538462,-0.246153846153846,
-0.230769230769231,-0.215384615384615,-0.2,-0.184615384615385,-0.169230769230769,
-0.153846153846154,-0.138461538461538,-0.123076923076923,-0.107692307692308,
-0.0923076923076923,-0.0769230769230769,-0.0615384615384615,-0.0461538461538462,
-0.0307692307692308,-0.0153846153846154,0.),(-1.,1.),.UNSPECIFIED.)
GEOMETRIC_REPRESENTATION_ITEM()
RATIONAL_B_SPLINE_SURFACE(((1.,1.),(1.,1.),(1.,1.),(1.,1.),(1.,1.),(1.,
1.),(1.,1.),(1.,1.),(1.,1.),(1.,1.),(1.,1.),(1.,1.),(1.,1.),(1.,1.),(1.,
1.),(1.,1.),(1.,1.),(1.,1.),(1.,1.),(1.,1.),(1.,1.),(1.,1.),(1.,1.),(1.,
1.),(1.,1.),(1.,1.),(1.,1.),(1.,1.),(1.,1.),(1.,1.),(1.,1.),(1.,1.),(1.,
1.),(1.,1.),(1.,1.),(1.,1.),(1.,1.),(1.,1.),(1.,1.),(1.,1.),(1.,1.),(1.,
1.),(1.,1.),(1.,1.),(1.,1.),(1.,1.),(1.,1.),(1.,1.),(1.,1.),(1.,1.),(1.,
1.),(1.,1.),(1.,1.),(1.,1.),(1.,1.),(1.,1.),(1.,1.),(1.,1.),(1.,1.),(1.,
1.),(1.,1.),(1.,1.),(1.,1.),(1.,1.),(1.,1.),(1.,1.),(1.,1.),(1.,1.),(1.,
1.),(1.,1.)))
REPRESENTATION_ITEM('')
SURFACE()
);
#27=(
BOUNDED_SURFACE()
B_SPLINE_SURFACE(5,1,((#29236,#29237),(#29238,#29239),(#29240,#29241),(#29242,
#29243),(#29244,#29245),(#29246,#29247),(#29248,#29249),(#29250,#29251),
(#29252,#29253),(#29254,#29255),(#29256,#29257),(#29258,#29259),(#29260,
#29261),(#29262,#29263),(#29264,#29265),(#29266,#29267),(#29268,#29269),
(#29270,#29271),(#29272,#29273),(#29274,#29275),(#29276,#29277),(#29278,
#29279),(#29280,#29281),(#29282,#29283),(#29284,#29285),(#29286,#29287),
(#29288,#29289),(#29290,#29291),(#29292,#29293),(#29294,#29295),(#29296,
#29297),(#29298,#29299),(#29300,#29301),(#29302,#29303),(#29304,#29305),
(#29306,#29307),(#29308,#29309),(#29310,#29311),(#29312,#29313),(#29314,
#29315),(#29316,#29317),(#29318,#29319),(#29320,#29321),(#29322,#29323),
(#29324,#29325),(#29326,#29327),(#29328,#29329),(#29330,#29331),(#29332,
#29333),(#29334,#29335),(#29336,#29337),(#29338,#29339),(#29340,#29341),
(#29342,#29343),(#29344,#29345),(#29346,#29347),(#29348,#29349),(#29350,
#29351),(#29352,#29353),(#29354,#29355),(#29356,#29357),(#29358,#29359),
(#29360,#29361),(#29362,#29363),(#29364,#29365),(#29366,#29367),(#29368,
#29369),(#29370,#29371),(#29372,#29373),(#29374,#29375)),.UNSPECIFIED.,
 .F.,.F.,.F.)
B_SPLINE_SURFACE_WITH_KNOTS((6,1,1,1,1,1,1,1,1,1,1,1,1,1,1,1,1,1,1,1,1,
1,1,1,1,1,1,1,1,1,1,1,1,1,1,1,1,1,1,1,1,1,1,1,1,1,1,1,1,1,1,1,1,1,1,1,1,
1,1,1,1,1,1,1,1,6),(2,2),(-1.,-0.984615384615383,-0.969230769230768,-0.953846153846152,
-0.938461538461537,-0.923076923076922,-0.907692307692306,-0.892307692307691,
-0.876923076923076,-0.86153846153846,-0.846153846153845,-0.83076923076923,
-0.815384615384614,-0.799999999999999,-0.784615384615384,-0.769230769230768,
-0.753846153846153,-0.738461538461538,-0.723076923076922,-0.707692307692307,
-0.692307692307692,-0.676923076923076,-0.661538461538461,-0.646153846153846,
-0.63076923076923,-0.615384615384615,-0.6,-0.584615384615384,-0.569230769230769,
-0.553846153846154,-0.538461538461538,-0.523076923076923,-0.507692307692308,
-0.492307692307692,-0.476923076923077,-0.461538461538462,-0.446153846153846,
-0.430769230769231,-0.415384615384615,-0.4,-0.384615384615385,-0.369230769230769,
-0.353846153846154,-0.338461538461538,-0.323076923076923,-0.307692307692308,
-0.292307692307692,-0.276923076923077,-0.261538461538462,-0.246153846153846,
-0.230769230769231,-0.215384615384615,-0.2,-0.184615384615385,-0.169230769230769,
-0.153846153846154,-0.138461538461538,-0.123076923076923,-0.107692307692308,
-0.0923076923076923,-0.0769230769230769,-0.0615384615384615,-0.0461538461538462,
-0.0307692307692308,-0.0153846153846154,0.),(-1.,1.),.UNSPECIFIED.)
GEOMETRIC_REPRESENTATION_ITEM()
RATIONAL_B_SPLINE_SURFACE(((1.,1.),(1.,1.),(1.,1.),(1.,1.),(1.,1.),(1.,
1.),(1.,1.),(1.,1.),(1.,1.),(1.,1.),(1.,1.),(1.,1.),(1.,1.),(1.,1.),(1.,
1.),(1.,1.),(1.,1.),(1.,1.),(1.,1.),(1.,1.),(1.,1.),(1.,1.),(1.,1.),(1.,
1.),(1.,1.),(1.,1.),(1.,1.),(1.,1.),(1.,1.),(1.,1.),(1.,1.),(1.,1.),(1.,
1.),(1.,1.),(1.,1.),(1.,1.),(1.,1.),(1.,1.),(1.,1.),(1.,1.),(1.,1.),(1.,
1.),(1.,1.),(1.,1.),(1.,1.),(1.,1.),(1.,1.),(1.,1.),(1.,1.),(1.,1.),(1.,
1.),(1.,1.),(1.,1.),(1.,1.),(1.,1.),(1.,1.),(1.,1.),(1.,1.),(1.,1.),(1.,
1.),(1.,1.),(1.,1.),(1.,1.),(1.,1.),(1.,1.),(1.,1.),(1.,1.),(1.,1.),(1.,
1.),(1.,1.)))
REPRESENTATION_ITEM('')
SURFACE()
);
#28=(
BOUNDED_SURFACE()
B_SPLINE_SURFACE(5,1,((#29452,#29453),(#29454,#29455),(#29456,#29457),(#29458,
#29459),(#29460,#29461),(#29462,#29463),(#29464,#29465),(#29466,#29467),
(#29468,#29469),(#29470,#29471),(#29472,#29473),(#29474,#29475),(#29476,
#29477),(#29478,#29479),(#29480,#29481),(#29482,#29483),(#29484,#29485),
(#29486,#29487),(#29488,#29489),(#29490,#29491),(#29492,#29493),(#29494,
#29495),(#29496,#29497),(#29498,#29499),(#29500,#29501),(#29502,#29503),
(#29504,#29505),(#29506,#29507),(#29508,#29509),(#29510,#29511),(#29512,
#29513),(#29514,#29515),(#29516,#29517),(#29518,#29519),(#29520,#29521),
(#29522,#29523),(#29524,#29525),(#29526,#29527),(#29528,#29529),(#29530,
#29531),(#29532,#29533),(#29534,#29535),(#29536,#29537),(#29538,#29539),
(#29540,#29541),(#29542,#29543),(#29544,#29545),(#29546,#29547),(#29548,
#29549),(#29550,#29551),(#29552,#29553),(#29554,#29555),(#29556,#29557),
(#29558,#29559),(#29560,#29561),(#29562,#29563),(#29564,#29565),(#29566,
#29567),(#29568,#29569),(#29570,#29571),(#29572,#29573),(#29574,#29575),
(#29576,#29577),(#29578,#29579),(#29580,#29581),(#29582,#29583),(#29584,
#29585),(#29586,#29587),(#29588,#29589),(#29590,#29591)),.UNSPECIFIED.,
 .F.,.F.,.F.)
B_SPLINE_SURFACE_WITH_KNOTS((6,1,1,1,1,1,1,1,1,1,1,1,1,1,1,1,1,1,1,1,1,
1,1,1,1,1,1,1,1,1,1,1,1,1,1,1,1,1,1,1,1,1,1,1,1,1,1,1,1,1,1,1,1,1,1,1,1,
1,1,1,1,1,1,1,1,6),(2,2),(-1.,-0.984615384615383,-0.969230769230768,-0.953846153846152,
-0.938461538461537,-0.923076923076922,-0.907692307692306,-0.892307692307691,
-0.876923076923076,-0.86153846153846,-0.846153846153845,-0.83076923076923,
-0.815384615384614,-0.799999999999999,-0.784615384615384,-0.769230769230768,
-0.753846153846153,-0.738461538461538,-0.723076923076922,-0.707692307692307,
-0.692307692307692,-0.676923076923076,-0.661538461538461,-0.646153846153846,
-0.63076923076923,-0.615384615384615,-0.6,-0.584615384615384,-0.569230769230769,
-0.553846153846154,-0.538461538461538,-0.523076923076923,-0.507692307692308,
-0.492307692307692,-0.476923076923077,-0.461538461538462,-0.446153846153846,
-0.430769230769231,-0.415384615384615,-0.4,-0.384615384615385,-0.369230769230769,
-0.353846153846154,-0.338461538461538,-0.323076923076923,-0.307692307692308,
-0.292307692307692,-0.276923076923077,-0.261538461538462,-0.246153846153846,
-0.230769230769231,-0.215384615384615,-0.2,-0.184615384615385,-0.169230769230769,
-0.153846153846154,-0.138461538461538,-0.123076923076923,-0.107692307692308,
-0.0923076923076923,-0.0769230769230769,-0.0615384615384615,-0.0461538461538462,
-0.0307692307692308,-0.0153846153846154,0.),(-1.,1.),.UNSPECIFIED.)
GEOMETRIC_REPRESENTATION_ITEM()
RATIONAL_B_SPLINE_SURFACE(((1.,1.),(1.,1.),(1.,1.),(1.,1.),(1.,1.),(1.,
1.),(1.,1.),(1.,1.),(1.,1.),(1.,1.),(1.,1.),(1.,1.),(1.,1.),(1.,1.),(1.,
1.),(1.,1.),(1.,1.),(1.,1.),(1.,1.),(1.,1.),(1.,1.),(1.,1.),(1.,1.),(1.,
1.),(1.,1.),(1.,1.),(1.,1.),(1.,1.),(1.,1.),(1.,1.),(1.,1.),(1.,1.),(1.,
1.),(1.,1.),(1.,1.),(1.,1.),(1.,1.),(1.,1.),(1.,1.),(1.,1.),(1.,1.),(1.,
1.),(1.,1.),(1.,1.),(1.,1.),(1.,1.),(1.,1.),(1.,1.),(1.,1.),(1.,1.),(1.,
1.),(1.,1.),(1.,1.),(1.,1.),(1.,1.),(1.,1.),(1.,1.),(1.,1.),(1.,1.),(1.,
1.),(1.,1.),(1.,1.),(1.,1.),(1.,1.),(1.,1.),(1.,1.),(1.,1.),(1.,1.),(1.,
1.),(1.,1.)))
REPRESENTATION_ITEM('')
SURFACE()
);
#29=(
BOUNDED_SURFACE()
B_SPLINE_SURFACE(5,1,((#29668,#29669),(#29670,#29671),(#29672,#29673),(#29674,
#29675),(#29676,#29677),(#29678,#29679),(#29680,#29681),(#29682,#29683),
(#29684,#29685),(#29686,#29687),(#29688,#29689),(#29690,#29691),(#29692,
#29693),(#29694,#29695),(#29696,#29697),(#29698,#29699),(#29700,#29701),
(#29702,#29703),(#29704,#29705),(#29706,#29707),(#29708,#29709),(#29710,
#29711),(#29712,#29713),(#29714,#29715),(#29716,#29717),(#29718,#29719),
(#29720,#29721),(#29722,#29723),(#29724,#29725),(#29726,#29727),(#29728,
#29729),(#29730,#29731),(#29732,#29733),(#29734,#29735),(#29736,#29737),
(#29738,#29739),(#29740,#29741),(#29742,#29743),(#29744,#29745),(#29746,
#29747),(#29748,#29749),(#29750,#29751),(#29752,#29753),(#29754,#29755),
(#29756,#29757),(#29758,#29759),(#29760,#29761),(#29762,#29763),(#29764,
#29765),(#29766,#29767),(#29768,#29769),(#29770,#29771),(#29772,#29773),
(#29774,#29775),(#29776,#29777),(#29778,#29779),(#29780,#29781),(#29782,
#29783),(#29784,#29785),(#29786,#29787),(#29788,#29789),(#29790,#29791),
(#29792,#29793),(#29794,#29795),(#29796,#29797),(#29798,#29799),(#29800,
#29801),(#29802,#29803),(#29804,#29805),(#29806,#29807)),.UNSPECIFIED.,
 .F.,.F.,.F.)
B_SPLINE_SURFACE_WITH_KNOTS((6,1,1,1,1,1,1,1,1,1,1,1,1,1,1,1,1,1,1,1,1,
1,1,1,1,1,1,1,1,1,1,1,1,1,1,1,1,1,1,1,1,1,1,1,1,1,1,1,1,1,1,1,1,1,1,1,1,
1,1,1,1,1,1,1,1,6),(2,2),(-1.,-0.984615384615383,-0.969230769230768,-0.953846153846152,
-0.938461538461537,-0.923076923076922,-0.907692307692306,-0.892307692307691,
-0.876923076923076,-0.86153846153846,-0.846153846153845,-0.83076923076923,
-0.815384615384614,-0.799999999999999,-0.784615384615384,-0.769230769230768,
-0.753846153846153,-0.738461538461538,-0.723076923076922,-0.707692307692307,
-0.692307692307692,-0.676923076923076,-0.661538461538461,-0.646153846153846,
-0.63076923076923,-0.615384615384615,-0.6,-0.584615384615384,-0.569230769230769,
-0.553846153846154,-0.538461538461538,-0.523076923076923,-0.507692307692308,
-0.492307692307692,-0.476923076923077,-0.461538461538462,-0.446153846153846,
-0.430769230769231,-0.415384615384615,-0.4,-0.384615384615385,-0.369230769230769,
-0.353846153846154,-0.338461538461538,-0.323076923076923,-0.307692307692308,
-0.292307692307692,-0.276923076923077,-0.261538461538462,-0.246153846153846,
-0.230769230769231,-0.215384615384615,-0.2,-0.184615384615385,-0.169230769230769,
-0.153846153846154,-0.138461538461538,-0.123076923076923,-0.107692307692308,
-0.0923076923076923,-0.0769230769230769,-0.0615384615384615,-0.0461538461538462,
-0.0307692307692308,-0.0153846153846154,0.),(-1.,1.),.UNSPECIFIED.)
GEOMETRIC_REPRESENTATION_ITEM()
RATIONAL_B_SPLINE_SURFACE(((1.,1.),(1.,1.),(1.,1.),(1.,1.),(1.,1.),(1.,
1.),(1.,1.),(1.,1.),(1.,1.),(1.,1.),(1.,1.),(1.,1.),(1.,1.),(1.,1.),(1.,
1.),(1.,1.),(1.,1.),(1.,1.),(1.,1.),(1.,1.),(1.,1.),(1.,1.),(1.,1.),(1.,
1.),(1.,1.),(1.,1.),(1.,1.),(1.,1.),(1.,1.),(1.,1.),(1.,1.),(1.,1.),(1.,
1.),(1.,1.),(1.,1.),(1.,1.),(1.,1.),(1.,1.),(1.,1.),(1.,1.),(1.,1.),(1.,
1.),(1.,1.),(1.,1.),(1.,1.),(1.,1.),(1.,1.),(1.,1.),(1.,1.),(1.,1.),(1.,
1.),(1.,1.),(1.,1.),(1.,1.),(1.,1.),(1.,1.),(1.,1.),(1.,1.),(1.,1.),(1.,
1.),(1.,1.),(1.,1.),(1.,1.),(1.,1.),(1.,1.),(1.,1.),(1.,1.),(1.,1.),(1.,
1.),(1.,1.)))
REPRESENTATION_ITEM('')
SURFACE()
);
#30=(
BOUNDED_SURFACE()
B_SPLINE_SURFACE(5,1,((#29884,#29885),(#29886,#29887),(#29888,#29889),(#29890,
#29891),(#29892,#29893),(#29894,#29895),(#29896,#29897),(#29898,#29899),
(#29900,#29901),(#29902,#29903),(#29904,#29905),(#29906,#29907),(#29908,
#29909),(#29910,#29911),(#29912,#29913),(#29914,#29915),(#29916,#29917),
(#29918,#29919),(#29920,#29921),(#29922,#29923),(#29924,#29925),(#29926,
#29927),(#29928,#29929),(#29930,#29931),(#29932,#29933),(#29934,#29935),
(#29936,#29937),(#29938,#29939),(#29940,#29941),(#29942,#29943),(#29944,
#29945),(#29946,#29947),(#29948,#29949),(#29950,#29951),(#29952,#29953),
(#29954,#29955),(#29956,#29957),(#29958,#29959),(#29960,#29961),(#29962,
#29963),(#29964,#29965),(#29966,#29967),(#29968,#29969),(#29970,#29971),
(#29972,#29973),(#29974,#29975),(#29976,#29977),(#29978,#29979),(#29980,
#29981),(#29982,#29983),(#29984,#29985),(#29986,#29987),(#29988,#29989),
(#29990,#29991),(#29992,#29993),(#29994,#29995),(#29996,#29997),(#29998,
#29999),(#30000,#30001),(#30002,#30003),(#30004,#30005),(#30006,#30007),
(#30008,#30009),(#30010,#30011),(#30012,#30013),(#30014,#30015),(#30016,
#30017),(#30018,#30019),(#30020,#30021),(#30022,#30023)),.UNSPECIFIED.,
 .F.,.F.,.F.)
B_SPLINE_SURFACE_WITH_KNOTS((6,1,1,1,1,1,1,1,1,1,1,1,1,1,1,1,1,1,1,1,1,
1,1,1,1,1,1,1,1,1,1,1,1,1,1,1,1,1,1,1,1,1,1,1,1,1,1,1,1,1,1,1,1,1,1,1,1,
1,1,1,1,1,1,1,1,6),(2,2),(-1.,-0.984615384615383,-0.969230769230768,-0.953846153846152,
-0.938461538461537,-0.923076923076922,-0.907692307692306,-0.892307692307691,
-0.876923076923076,-0.86153846153846,-0.846153846153845,-0.83076923076923,
-0.815384615384614,-0.799999999999999,-0.784615384615384,-0.769230769230768,
-0.753846153846153,-0.738461538461538,-0.723076923076922,-0.707692307692307,
-0.692307692307692,-0.676923076923076,-0.661538461538461,-0.646153846153846,
-0.63076923076923,-0.615384615384615,-0.6,-0.584615384615384,-0.569230769230769,
-0.553846153846154,-0.538461538461538,-0.523076923076923,-0.507692307692308,
-0.492307692307692,-0.476923076923077,-0.461538461538462,-0.446153846153846,
-0.430769230769231,-0.415384615384615,-0.4,-0.384615384615385,-0.369230769230769,
-0.353846153846154,-0.338461538461538,-0.323076923076923,-0.307692307692308,
-0.292307692307692,-0.276923076923077,-0.261538461538462,-0.246153846153846,
-0.230769230769231,-0.215384615384615,-0.2,-0.184615384615385,-0.169230769230769,
-0.153846153846154,-0.138461538461538,-0.123076923076923,-0.107692307692308,
-0.0923076923076923,-0.0769230769230769,-0.0615384615384615,-0.0461538461538462,
-0.0307692307692308,-0.0153846153846154,0.),(-1.,1.),.UNSPECIFIED.)
GEOMETRIC_REPRESENTATION_ITEM()
RATIONAL_B_SPLINE_SURFACE(((1.,1.),(1.,1.),(1.,1.),(1.,1.),(1.,1.),(1.,
1.),(1.,1.),(1.,1.),(1.,1.),(1.,1.),(1.,1.),(1.,1.),(1.,1.),(1.,1.),(1.,
1.),(1.,1.),(1.,1.),(1.,1.),(1.,1.),(1.,1.),(1.,1.),(1.,1.),(1.,1.),(1.,
1.),(1.,1.),(1.,1.),(1.,1.),(1.,1.),(1.,1.),(1.,1.),(1.,1.),(1.,1.),(1.,
1.),(1.,1.),(1.,1.),(1.,1.),(1.,1.),(1.,1.),(1.,1.),(1.,1.),(1.,1.),(1.,
1.),(1.,1.),(1.,1.),(1.,1.),(1.,1.),(1.,1.),(1.,1.),(1.,1.),(1.,1.),(1.,
1.),(1.,1.),(1.,1.),(1.,1.),(1.,1.),(1.,1.),(1.,1.),(1.,1.),(1.,1.),(1.,
1.),(1.,1.),(1.,1.),(1.,1.),(1.,1.),(1.,1.),(1.,1.),(1.,1.),(1.,1.),(1.,
1.),(1.,1.)))
REPRESENTATION_ITEM('')
SURFACE()
);
#31=(
BOUNDED_SURFACE()
B_SPLINE_SURFACE(5,1,((#30100,#30101),(#30102,#30103),(#30104,#30105),(#30106,
#30107),(#30108,#30109),(#30110,#30111),(#30112,#30113),(#30114,#30115),
(#30116,#30117),(#30118,#30119),(#30120,#30121),(#30122,#30123),(#30124,
#30125),(#30126,#30127),(#30128,#30129),(#30130,#30131),(#30132,#30133),
(#30134,#30135),(#30136,#30137),(#30138,#30139),(#30140,#30141),(#30142,
#30143),(#30144,#30145),(#30146,#30147),(#30148,#30149),(#30150,#30151),
(#30152,#30153),(#30154,#30155),(#30156,#30157),(#30158,#30159),(#30160,
#30161),(#30162,#30163),(#30164,#30165),(#30166,#30167),(#30168,#30169),
(#30170,#30171),(#30172,#30173),(#30174,#30175),(#30176,#30177),(#30178,
#30179),(#30180,#30181),(#30182,#30183),(#30184,#30185),(#30186,#30187),
(#30188,#30189),(#30190,#30191),(#30192,#30193),(#30194,#30195),(#30196,
#30197),(#30198,#30199),(#30200,#30201),(#30202,#30203),(#30204,#30205),
(#30206,#30207),(#30208,#30209),(#30210,#30211),(#30212,#30213),(#30214,
#30215),(#30216,#30217),(#30218,#30219),(#30220,#30221),(#30222,#30223),
(#30224,#30225),(#30226,#30227),(#30228,#30229),(#30230,#30231),(#30232,
#30233),(#30234,#30235),(#30236,#30237),(#30238,#30239)),.UNSPECIFIED.,
 .F.,.F.,.F.)
B_SPLINE_SURFACE_WITH_KNOTS((6,1,1,1,1,1,1,1,1,1,1,1,1,1,1,1,1,1,1,1,1,
1,1,1,1,1,1,1,1,1,1,1,1,1,1,1,1,1,1,1,1,1,1,1,1,1,1,1,1,1,1,1,1,1,1,1,1,
1,1,1,1,1,1,1,1,6),(2,2),(-1.,-0.984615384615383,-0.969230769230768,-0.953846153846152,
-0.938461538461537,-0.923076923076922,-0.907692307692306,-0.892307692307691,
-0.876923076923076,-0.86153846153846,-0.846153846153845,-0.83076923076923,
-0.815384615384614,-0.799999999999999,-0.784615384615384,-0.769230769230768,
-0.753846153846153,-0.738461538461538,-0.723076923076922,-0.707692307692307,
-0.692307692307692,-0.676923076923076,-0.661538461538461,-0.646153846153846,
-0.63076923076923,-0.615384615384615,-0.6,-0.584615384615384,-0.569230769230769,
-0.553846153846154,-0.538461538461538,-0.523076923076923,-0.507692307692308,
-0.492307692307692,-0.476923076923077,-0.461538461538462,-0.446153846153846,
-0.430769230769231,-0.415384615384615,-0.4,-0.384615384615385,-0.369230769230769,
-0.353846153846154,-0.338461538461538,-0.323076923076923,-0.307692307692308,
-0.292307692307692,-0.276923076923077,-0.261538461538462,-0.246153846153846,
-0.230769230769231,-0.215384615384615,-0.2,-0.184615384615385,-0.169230769230769,
-0.153846153846154,-0.138461538461538,-0.123076923076923,-0.107692307692308,
-0.0923076923076923,-0.0769230769230769,-0.0615384615384615,-0.0461538461538462,
-0.0307692307692308,-0.0153846153846154,0.),(-1.,1.),.UNSPECIFIED.)
GEOMETRIC_REPRESENTATION_ITEM()
RATIONAL_B_SPLINE_SURFACE(((1.,1.),(1.,1.),(1.,1.),(1.,1.),(1.,1.),(1.,
1.),(1.,1.),(1.,1.),(1.,1.),(1.,1.),(1.,1.),(1.,1.),(1.,1.),(1.,1.),(1.,
1.),(1.,1.),(1.,1.),(1.,1.),(1.,1.),(1.,1.),(1.,1.),(1.,1.),(1.,1.),(1.,
1.),(1.,1.),(1.,1.),(1.,1.),(1.,1.),(1.,1.),(1.,1.),(1.,1.),(1.,1.),(1.,
1.),(1.,1.),(1.,1.),(1.,1.),(1.,1.),(1.,1.),(1.,1.),(1.,1.),(1.,1.),(1.,
1.),(1.,1.),(1.,1.),(1.,1.),(1.,1.),(1.,1.),(1.,1.),(1.,1.),(1.,1.),(1.,
1.),(1.,1.),(1.,1.),(1.,1.),(1.,1.),(1.,1.),(1.,1.),(1.,1.),(1.,1.),(1.,
1.),(1.,1.),(1.,1.),(1.,1.),(1.,1.),(1.,1.),(1.,1.),(1.,1.),(1.,1.),(1.,
1.),(1.,1.)))
REPRESENTATION_ITEM('')
SURFACE()
);
#32=(
BOUNDED_SURFACE()
B_SPLINE_SURFACE(5,1,((#30316,#30317),(#30318,#30319),(#30320,#30321),(#30322,
#30323),(#30324,#30325),(#30326,#30327),(#30328,#30329),(#30330,#30331),
(#30332,#30333),(#30334,#30335),(#30336,#30337),(#30338,#30339),(#30340,
#30341),(#30342,#30343),(#30344,#30345),(#30346,#30347),(#30348,#30349),
(#30350,#30351),(#30352,#30353),(#30354,#30355),(#30356,#30357),(#30358,
#30359),(#30360,#30361),(#30362,#30363),(#30364,#30365),(#30366,#30367),
(#30368,#30369),(#30370,#30371),(#30372,#30373),(#30374,#30375),(#30376,
#30377),(#30378,#30379),(#30380,#30381),(#30382,#30383),(#30384,#30385),
(#30386,#30387),(#30388,#30389),(#30390,#30391),(#30392,#30393),(#30394,
#30395),(#30396,#30397),(#30398,#30399),(#30400,#30401),(#30402,#30403),
(#30404,#30405),(#30406,#30407),(#30408,#30409),(#30410,#30411),(#30412,
#30413),(#30414,#30415),(#30416,#30417),(#30418,#30419),(#30420,#30421),
(#30422,#30423),(#30424,#30425),(#30426,#30427),(#30428,#30429),(#30430,
#30431),(#30432,#30433),(#30434,#30435),(#30436,#30437),(#30438,#30439),
(#30440,#30441),(#30442,#30443),(#30444,#30445),(#30446,#30447),(#30448,
#30449),(#30450,#30451),(#30452,#30453),(#30454,#30455)),.UNSPECIFIED.,
 .F.,.F.,.F.)
B_SPLINE_SURFACE_WITH_KNOTS((6,1,1,1,1,1,1,1,1,1,1,1,1,1,1,1,1,1,1,1,1,
1,1,1,1,1,1,1,1,1,1,1,1,1,1,1,1,1,1,1,1,1,1,1,1,1,1,1,1,1,1,1,1,1,1,1,1,
1,1,1,1,1,1,1,1,6),(2,2),(-1.,-0.984615384615383,-0.969230769230768,-0.953846153846152,
-0.938461538461537,-0.923076923076922,-0.907692307692306,-0.892307692307691,
-0.876923076923076,-0.86153846153846,-0.846153846153845,-0.83076923076923,
-0.815384615384614,-0.799999999999999,-0.784615384615384,-0.769230769230768,
-0.753846153846153,-0.738461538461538,-0.723076923076922,-0.707692307692307,
-0.692307692307692,-0.676923076923076,-0.661538461538461,-0.646153846153846,
-0.63076923076923,-0.615384615384615,-0.6,-0.584615384615384,-0.569230769230769,
-0.553846153846154,-0.538461538461538,-0.523076923076923,-0.507692307692308,
-0.492307692307692,-0.476923076923077,-0.461538461538462,-0.446153846153846,
-0.430769230769231,-0.415384615384615,-0.4,-0.384615384615385,-0.369230769230769,
-0.353846153846154,-0.338461538461538,-0.323076923076923,-0.307692307692308,
-0.292307692307692,-0.276923076923077,-0.261538461538462,-0.246153846153846,
-0.230769230769231,-0.215384615384615,-0.2,-0.184615384615385,-0.169230769230769,
-0.153846153846154,-0.138461538461538,-0.123076923076923,-0.107692307692308,
-0.0923076923076923,-0.0769230769230769,-0.0615384615384615,-0.0461538461538462,
-0.0307692307692308,-0.0153846153846154,0.),(-1.,1.),.UNSPECIFIED.)
GEOMETRIC_REPRESENTATION_ITEM()
RATIONAL_B_SPLINE_SURFACE(((1.,1.),(1.,1.),(1.,1.),(1.,1.),(1.,1.),(1.,
1.),(1.,1.),(1.,1.),(1.,1.),(1.,1.),(1.,1.),(1.,1.),(1.,1.),(1.,1.),(1.,
1.),(1.,1.),(1.,1.),(1.,1.),(1.,1.),(1.,1.),(1.,1.),(1.,1.),(1.,1.),(1.,
1.),(1.,1.),(1.,1.),(1.,1.),(1.,1.),(1.,1.),(1.,1.),(1.,1.),(1.,1.),(1.,
1.),(1.,1.),(1.,1.),(1.,1.),(1.,1.),(1.,1.),(1.,1.),(1.,1.),(1.,1.),(1.,
1.),(1.,1.),(1.,1.),(1.,1.),(1.,1.),(1.,1.),(1.,1.),(1.,1.),(1.,1.),(1.,
1.),(1.,1.),(1.,1.),(1.,1.),(1.,1.),(1.,1.),(1.,1.),(1.,1.),(1.,1.),(1.,
1.),(1.,1.),(1.,1.),(1.,1.),(1.,1.),(1.,1.),(1.,1.),(1.,1.),(1.,1.),(1.,
1.),(1.,1.)))
REPRESENTATION_ITEM('')
SURFACE()
);
#33=(
BOUNDED_SURFACE()
B_SPLINE_SURFACE(5,1,((#30532,#30533),(#30534,#30535),(#30536,#30537),(#30538,
#30539),(#30540,#30541),(#30542,#30543),(#30544,#30545),(#30546,#30547),
(#30548,#30549),(#30550,#30551),(#30552,#30553),(#30554,#30555),(#30556,
#30557),(#30558,#30559),(#30560,#30561),(#30562,#30563),(#30564,#30565),
(#30566,#30567),(#30568,#30569),(#30570,#30571),(#30572,#30573),(#30574,
#30575),(#30576,#30577),(#30578,#30579),(#30580,#30581),(#30582,#30583),
(#30584,#30585),(#30586,#30587),(#30588,#30589),(#30590,#30591),(#30592,
#30593),(#30594,#30595),(#30596,#30597),(#30598,#30599),(#30600,#30601),
(#30602,#30603),(#30604,#30605),(#30606,#30607),(#30608,#30609),(#30610,
#30611),(#30612,#30613),(#30614,#30615),(#30616,#30617),(#30618,#30619),
(#30620,#30621),(#30622,#30623),(#30624,#30625),(#30626,#30627),(#30628,
#30629),(#30630,#30631),(#30632,#30633),(#30634,#30635),(#30636,#30637),
(#30638,#30639),(#30640,#30641),(#30642,#30643),(#30644,#30645),(#30646,
#30647),(#30648,#30649),(#30650,#30651),(#30652,#30653),(#30654,#30655),
(#30656,#30657),(#30658,#30659),(#30660,#30661),(#30662,#30663),(#30664,
#30665),(#30666,#30667),(#30668,#30669),(#30670,#30671)),.UNSPECIFIED.,
 .F.,.F.,.F.)
B_SPLINE_SURFACE_WITH_KNOTS((6,1,1,1,1,1,1,1,1,1,1,1,1,1,1,1,1,1,1,1,1,
1,1,1,1,1,1,1,1,1,1,1,1,1,1,1,1,1,1,1,1,1,1,1,1,1,1,1,1,1,1,1,1,1,1,1,1,
1,1,1,1,1,1,1,1,6),(2,2),(-1.,-0.984615384615383,-0.969230769230768,-0.953846153846152,
-0.938461538461537,-0.923076923076922,-0.907692307692306,-0.892307692307691,
-0.876923076923076,-0.86153846153846,-0.846153846153845,-0.83076923076923,
-0.815384615384614,-0.799999999999999,-0.784615384615384,-0.769230769230768,
-0.753846153846153,-0.738461538461538,-0.723076923076922,-0.707692307692307,
-0.692307692307692,-0.676923076923076,-0.661538461538461,-0.646153846153846,
-0.63076923076923,-0.615384615384615,-0.6,-0.584615384615384,-0.569230769230769,
-0.553846153846154,-0.538461538461538,-0.523076923076923,-0.507692307692308,
-0.492307692307692,-0.476923076923077,-0.461538461538462,-0.446153846153846,
-0.430769230769231,-0.415384615384615,-0.4,-0.384615384615385,-0.369230769230769,
-0.353846153846154,-0.338461538461538,-0.323076923076923,-0.307692307692308,
-0.292307692307692,-0.276923076923077,-0.261538461538462,-0.246153846153846,
-0.230769230769231,-0.215384615384615,-0.2,-0.184615384615385,-0.169230769230769,
-0.153846153846154,-0.138461538461538,-0.123076923076923,-0.107692307692308,
-0.0923076923076923,-0.0769230769230769,-0.0615384615384615,-0.0461538461538462,
-0.0307692307692308,-0.0153846153846154,0.),(-1.,1.),.UNSPECIFIED.)
GEOMETRIC_REPRESENTATION_ITEM()
RATIONAL_B_SPLINE_SURFACE(((1.,1.),(1.,1.),(1.,1.),(1.,1.),(1.,1.),(1.,
1.),(1.,1.),(1.,1.),(1.,1.),(1.,1.),(1.,1.),(1.,1.),(1.,1.),(1.,1.),(1.,
1.),(1.,1.),(1.,1.),(1.,1.),(1.,1.),(1.,1.),(1.,1.),(1.,1.),(1.,1.),(1.,
1.),(1.,1.),(1.,1.),(1.,1.),(1.,1.),(1.,1.),(1.,1.),(1.,1.),(1.,1.),(1.,
1.),(1.,1.),(1.,1.),(1.,1.),(1.,1.),(1.,1.),(1.,1.),(1.,1.),(1.,1.),(1.,
1.),(1.,1.),(1.,1.),(1.,1.),(1.,1.),(1.,1.),(1.,1.),(1.,1.),(1.,1.),(1.,
1.),(1.,1.),(1.,1.),(1.,1.),(1.,1.),(1.,1.),(1.,1.),(1.,1.),(1.,1.),(1.,
1.),(1.,1.),(1.,1.),(1.,1.),(1.,1.),(1.,1.),(1.,1.),(1.,1.),(1.,1.),(1.,
1.),(1.,1.)))
REPRESENTATION_ITEM('')
SURFACE()
);
#34=(
BOUNDED_SURFACE()
B_SPLINE_SURFACE(5,1,((#30748,#30749),(#30750,#30751),(#30752,#30753),(#30754,
#30755),(#30756,#30757),(#30758,#30759),(#30760,#30761),(#30762,#30763),
(#30764,#30765),(#30766,#30767),(#30768,#30769),(#30770,#30771),(#30772,
#30773),(#30774,#30775),(#30776,#30777),(#30778,#30779),(#30780,#30781),
(#30782,#30783),(#30784,#30785),(#30786,#30787),(#30788,#30789),(#30790,
#30791),(#30792,#30793),(#30794,#30795),(#30796,#30797),(#30798,#30799),
(#30800,#30801),(#30802,#30803),(#30804,#30805),(#30806,#30807),(#30808,
#30809),(#30810,#30811),(#30812,#30813),(#30814,#30815),(#30816,#30817),
(#30818,#30819),(#30820,#30821),(#30822,#30823),(#30824,#30825),(#30826,
#30827),(#30828,#30829),(#30830,#30831),(#30832,#30833),(#30834,#30835),
(#30836,#30837),(#30838,#30839),(#30840,#30841),(#30842,#30843),(#30844,
#30845),(#30846,#30847),(#30848,#30849),(#30850,#30851),(#30852,#30853),
(#30854,#30855),(#30856,#30857),(#30858,#30859),(#30860,#30861),(#30862,
#30863),(#30864,#30865),(#30866,#30867),(#30868,#30869),(#30870,#30871),
(#30872,#30873),(#30874,#30875),(#30876,#30877),(#30878,#30879),(#30880,
#30881),(#30882,#30883),(#30884,#30885),(#30886,#30887)),.UNSPECIFIED.,
 .F.,.F.,.F.)
B_SPLINE_SURFACE_WITH_KNOTS((6,1,1,1,1,1,1,1,1,1,1,1,1,1,1,1,1,1,1,1,1,
1,1,1,1,1,1,1,1,1,1,1,1,1,1,1,1,1,1,1,1,1,1,1,1,1,1,1,1,1,1,1,1,1,1,1,1,
1,1,1,1,1,1,1,1,6),(2,2),(-1.,-0.984615384615383,-0.969230769230768,-0.953846153846152,
-0.938461538461537,-0.923076923076922,-0.907692307692306,-0.892307692307691,
-0.876923076923076,-0.86153846153846,-0.846153846153845,-0.83076923076923,
-0.815384615384614,-0.799999999999999,-0.784615384615384,-0.769230769230768,
-0.753846153846153,-0.738461538461538,-0.723076923076922,-0.707692307692307,
-0.692307692307692,-0.676923076923076,-0.661538461538461,-0.646153846153846,
-0.63076923076923,-0.615384615384615,-0.6,-0.584615384615384,-0.569230769230769,
-0.553846153846154,-0.538461538461538,-0.523076923076923,-0.507692307692308,
-0.492307692307692,-0.476923076923077,-0.461538461538462,-0.446153846153846,
-0.430769230769231,-0.415384615384615,-0.4,-0.384615384615385,-0.369230769230769,
-0.353846153846154,-0.338461538461538,-0.323076923076923,-0.307692307692308,
-0.292307692307692,-0.276923076923077,-0.261538461538462,-0.246153846153846,
-0.230769230769231,-0.215384615384615,-0.2,-0.184615384615385,-0.169230769230769,
-0.153846153846154,-0.138461538461538,-0.123076923076923,-0.107692307692308,
-0.0923076923076923,-0.0769230769230769,-0.0615384615384615,-0.0461538461538462,
-0.0307692307692308,-0.0153846153846154,0.),(-1.,1.),.UNSPECIFIED.)
GEOMETRIC_REPRESENTATION_ITEM()
RATIONAL_B_SPLINE_SURFACE(((1.,1.),(1.,1.),(1.,1.),(1.,1.),(1.,1.),(1.,
1.),(1.,1.),(1.,1.),(1.,1.),(1.,1.),(1.,1.),(1.,1.),(1.,1.),(1.,1.),(1.,
1.),(1.,1.),(1.,1.),(1.,1.),(1.,1.),(1.,1.),(1.,1.),(1.,1.),(1.,1.),(1.,
1.),(1.,1.),(1.,1.),(1.,1.),(1.,1.),(1.,1.),(1.,1.),(1.,1.),(1.,1.),(1.,
1.),(1.,1.),(1.,1.),(1.,1.),(1.,1.),(1.,1.),(1.,1.),(1.,1.),(1.,1.),(1.,
1.),(1.,1.),(1.,1.),(1.,1.),(1.,1.),(1.,1.),(1.,1.),(1.,1.),(1.,1.),(1.,
1.),(1.,1.),(1.,1.),(1.,1.),(1.,1.),(1.,1.),(1.,1.),(1.,1.),(1.,1.),(1.,
1.),(1.,1.),(1.,1.),(1.,1.),(1.,1.),(1.,1.),(1.,1.),(1.,1.),(1.,1.),(1.,
1.),(1.,1.)))
REPRESENTATION_ITEM('')
SURFACE()
);
#35=(
BOUNDED_SURFACE()
B_SPLINE_SURFACE(5,1,((#30964,#30965),(#30966,#30967),(#30968,#30969),(#30970,
#30971),(#30972,#30973),(#30974,#30975),(#30976,#30977),(#30978,#30979),
(#30980,#30981),(#30982,#30983),(#30984,#30985),(#30986,#30987),(#30988,
#30989),(#30990,#30991),(#30992,#30993),(#30994,#30995),(#30996,#30997),
(#30998,#30999),(#31000,#31001),(#31002,#31003),(#31004,#31005),(#31006,
#31007),(#31008,#31009),(#31010,#31011),(#31012,#31013),(#31014,#31015),
(#31016,#31017),(#31018,#31019),(#31020,#31021),(#31022,#31023),(#31024,
#31025),(#31026,#31027),(#31028,#31029),(#31030,#31031),(#31032,#31033),
(#31034,#31035),(#31036,#31037),(#31038,#31039),(#31040,#31041),(#31042,
#31043),(#31044,#31045),(#31046,#31047),(#31048,#31049),(#31050,#31051),
(#31052,#31053),(#31054,#31055),(#31056,#31057),(#31058,#31059),(#31060,
#31061),(#31062,#31063),(#31064,#31065),(#31066,#31067),(#31068,#31069),
(#31070,#31071),(#31072,#31073),(#31074,#31075),(#31076,#31077),(#31078,
#31079),(#31080,#31081),(#31082,#31083),(#31084,#31085),(#31086,#31087),
(#31088,#31089),(#31090,#31091),(#31092,#31093),(#31094,#31095),(#31096,
#31097),(#31098,#31099),(#31100,#31101),(#31102,#31103)),.UNSPECIFIED.,
 .F.,.F.,.F.)
B_SPLINE_SURFACE_WITH_KNOTS((6,1,1,1,1,1,1,1,1,1,1,1,1,1,1,1,1,1,1,1,1,
1,1,1,1,1,1,1,1,1,1,1,1,1,1,1,1,1,1,1,1,1,1,1,1,1,1,1,1,1,1,1,1,1,1,1,1,
1,1,1,1,1,1,1,1,6),(2,2),(-1.,-0.984615384615383,-0.969230769230768,-0.953846153846152,
-0.938461538461537,-0.923076923076922,-0.907692307692306,-0.892307692307691,
-0.876923076923076,-0.86153846153846,-0.846153846153845,-0.83076923076923,
-0.815384615384614,-0.799999999999999,-0.784615384615384,-0.769230769230768,
-0.753846153846153,-0.738461538461538,-0.723076923076922,-0.707692307692307,
-0.692307692307692,-0.676923076923076,-0.661538461538461,-0.646153846153846,
-0.63076923076923,-0.615384615384615,-0.6,-0.584615384615384,-0.569230769230769,
-0.553846153846154,-0.538461538461538,-0.523076923076923,-0.507692307692308,
-0.492307692307692,-0.476923076923077,-0.461538461538462,-0.446153846153846,
-0.430769230769231,-0.415384615384615,-0.4,-0.384615384615385,-0.369230769230769,
-0.353846153846154,-0.338461538461538,-0.323076923076923,-0.307692307692308,
-0.292307692307692,-0.276923076923077,-0.261538461538462,-0.246153846153846,
-0.230769230769231,-0.215384615384615,-0.2,-0.184615384615385,-0.169230769230769,
-0.153846153846154,-0.138461538461538,-0.123076923076923,-0.107692307692308,
-0.0923076923076923,-0.0769230769230769,-0.0615384615384615,-0.0461538461538462,
-0.0307692307692308,-0.0153846153846154,0.),(-1.,1.),.UNSPECIFIED.)
GEOMETRIC_REPRESENTATION_ITEM()
RATIONAL_B_SPLINE_SURFACE(((1.,1.),(1.,1.),(1.,1.),(1.,1.),(1.,1.),(1.,
1.),(1.,1.),(1.,1.),(1.,1.),(1.,1.),(1.,1.),(1.,1.),(1.,1.),(1.,1.),(1.,
1.),(1.,1.),(1.,1.),(1.,1.),(1.,1.),(1.,1.),(1.,1.),(1.,1.),(1.,1.),(1.,
1.),(1.,1.),(1.,1.),(1.,1.),(1.,1.),(1.,1.),(1.,1.),(1.,1.),(1.,1.),(1.,
1.),(1.,1.),(1.,1.),(1.,1.),(1.,1.),(1.,1.),(1.,1.),(1.,1.),(1.,1.),(1.,
1.),(1.,1.),(1.,1.),(1.,1.),(1.,1.),(1.,1.),(1.,1.),(1.,1.),(1.,1.),(1.,
1.),(1.,1.),(1.,1.),(1.,1.),(1.,1.),(1.,1.),(1.,1.),(1.,1.),(1.,1.),(1.,
1.),(1.,1.),(1.,1.),(1.,1.),(1.,1.),(1.,1.),(1.,1.),(1.,1.),(1.,1.),(1.,
1.),(1.,1.)))
REPRESENTATION_ITEM('')
SURFACE()
);
#36=(
BOUNDED_SURFACE()
B_SPLINE_SURFACE(5,1,((#31180,#31181),(#31182,#31183),(#31184,#31185),(#31186,
#31187),(#31188,#31189),(#31190,#31191),(#31192,#31193),(#31194,#31195),
(#31196,#31197),(#31198,#31199),(#31200,#31201),(#31202,#31203),(#31204,
#31205),(#31206,#31207),(#31208,#31209),(#31210,#31211),(#31212,#31213),
(#31214,#31215),(#31216,#31217),(#31218,#31219),(#31220,#31221),(#31222,
#31223),(#31224,#31225),(#31226,#31227),(#31228,#31229),(#31230,#31231),
(#31232,#31233),(#31234,#31235),(#31236,#31237),(#31238,#31239),(#31240,
#31241),(#31242,#31243),(#31244,#31245),(#31246,#31247),(#31248,#31249),
(#31250,#31251),(#31252,#31253),(#31254,#31255),(#31256,#31257),(#31258,
#31259),(#31260,#31261),(#31262,#31263),(#31264,#31265),(#31266,#31267),
(#31268,#31269),(#31270,#31271),(#31272,#31273),(#31274,#31275),(#31276,
#31277),(#31278,#31279),(#31280,#31281),(#31282,#31283),(#31284,#31285),
(#31286,#31287),(#31288,#31289),(#31290,#31291),(#31292,#31293),(#31294,
#31295),(#31296,#31297),(#31298,#31299),(#31300,#31301),(#31302,#31303),
(#31304,#31305),(#31306,#31307),(#31308,#31309),(#31310,#31311),(#31312,
#31313),(#31314,#31315),(#31316,#31317),(#31318,#31319)),.UNSPECIFIED.,
 .F.,.F.,.F.)
B_SPLINE_SURFACE_WITH_KNOTS((6,1,1,1,1,1,1,1,1,1,1,1,1,1,1,1,1,1,1,1,1,
1,1,1,1,1,1,1,1,1,1,1,1,1,1,1,1,1,1,1,1,1,1,1,1,1,1,1,1,1,1,1,1,1,1,1,1,
1,1,1,1,1,1,1,1,6),(2,2),(-1.,-0.984615384615383,-0.969230769230768,-0.953846153846152,
-0.938461538461537,-0.923076923076922,-0.907692307692306,-0.892307692307691,
-0.876923076923076,-0.86153846153846,-0.846153846153845,-0.83076923076923,
-0.815384615384614,-0.799999999999999,-0.784615384615384,-0.769230769230768,
-0.753846153846153,-0.738461538461538,-0.723076923076922,-0.707692307692307,
-0.692307692307692,-0.676923076923076,-0.661538461538461,-0.646153846153846,
-0.63076923076923,-0.615384615384615,-0.6,-0.584615384615384,-0.569230769230769,
-0.553846153846154,-0.538461538461538,-0.523076923076923,-0.507692307692308,
-0.492307692307692,-0.476923076923077,-0.461538461538462,-0.446153846153846,
-0.430769230769231,-0.415384615384615,-0.4,-0.384615384615385,-0.369230769230769,
-0.353846153846154,-0.338461538461538,-0.323076923076923,-0.307692307692308,
-0.292307692307692,-0.276923076923077,-0.261538461538462,-0.246153846153846,
-0.230769230769231,-0.215384615384615,-0.2,-0.184615384615385,-0.169230769230769,
-0.153846153846154,-0.138461538461538,-0.123076923076923,-0.107692307692308,
-0.0923076923076923,-0.0769230769230769,-0.0615384615384615,-0.0461538461538462,
-0.0307692307692308,-0.0153846153846154,0.),(-1.,1.),.UNSPECIFIED.)
GEOMETRIC_REPRESENTATION_ITEM()
RATIONAL_B_SPLINE_SURFACE(((1.,1.),(1.,1.),(1.,1.),(1.,1.),(1.,1.),(1.,
1.),(1.,1.),(1.,1.),(1.,1.),(1.,1.),(1.,1.),(1.,1.),(1.,1.),(1.,1.),(1.,
1.),(1.,1.),(1.,1.),(1.,1.),(1.,1.),(1.,1.),(1.,1.),(1.,1.),(1.,1.),(1.,
1.),(1.,1.),(1.,1.),(1.,1.),(1.,1.),(1.,1.),(1.,1.),(1.,1.),(1.,1.),(1.,
1.),(1.,1.),(1.,1.),(1.,1.),(1.,1.),(1.,1.),(1.,1.),(1.,1.),(1.,1.),(1.,
1.),(1.,1.),(1.,1.),(1.,1.),(1.,1.),(1.,1.),(1.,1.),(1.,1.),(1.,1.),(1.,
1.),(1.,1.),(1.,1.),(1.,1.),(1.,1.),(1.,1.),(1.,1.),(1.,1.),(1.,1.),(1.,
1.),(1.,1.),(1.,1.),(1.,1.),(1.,1.),(1.,1.),(1.,1.),(1.,1.),(1.,1.),(1.,
1.),(1.,1.)))
REPRESENTATION_ITEM('')
SURFACE()
);
#37=(
BOUNDED_SURFACE()
B_SPLINE_SURFACE(5,1,((#31396,#31397),(#31398,#31399),(#31400,#31401),(#31402,
#31403),(#31404,#31405),(#31406,#31407),(#31408,#31409),(#31410,#31411),
(#31412,#31413),(#31414,#31415),(#31416,#31417),(#31418,#31419),(#31420,
#31421),(#31422,#31423),(#31424,#31425),(#31426,#31427),(#31428,#31429),
(#31430,#31431),(#31432,#31433),(#31434,#31435),(#31436,#31437),(#31438,
#31439),(#31440,#31441),(#31442,#31443),(#31444,#31445),(#31446,#31447),
(#31448,#31449),(#31450,#31451),(#31452,#31453),(#31454,#31455),(#31456,
#31457),(#31458,#31459),(#31460,#31461),(#31462,#31463),(#31464,#31465),
(#31466,#31467),(#31468,#31469),(#31470,#31471),(#31472,#31473),(#31474,
#31475),(#31476,#31477),(#31478,#31479),(#31480,#31481),(#31482,#31483),
(#31484,#31485),(#31486,#31487),(#31488,#31489),(#31490,#31491),(#31492,
#31493),(#31494,#31495),(#31496,#31497),(#31498,#31499),(#31500,#31501),
(#31502,#31503),(#31504,#31505),(#31506,#31507),(#31508,#31509),(#31510,
#31511),(#31512,#31513),(#31514,#31515),(#31516,#31517),(#31518,#31519),
(#31520,#31521),(#31522,#31523),(#31524,#31525),(#31526,#31527),(#31528,
#31529),(#31530,#31531),(#31532,#31533),(#31534,#31535)),.UNSPECIFIED.,
 .F.,.F.,.F.)
B_SPLINE_SURFACE_WITH_KNOTS((6,1,1,1,1,1,1,1,1,1,1,1,1,1,1,1,1,1,1,1,1,
1,1,1,1,1,1,1,1,1,1,1,1,1,1,1,1,1,1,1,1,1,1,1,1,1,1,1,1,1,1,1,1,1,1,1,1,
1,1,1,1,1,1,1,1,6),(2,2),(-1.,-0.984615384615383,-0.969230769230768,-0.953846153846152,
-0.938461538461537,-0.923076923076922,-0.907692307692306,-0.892307692307691,
-0.876923076923076,-0.86153846153846,-0.846153846153845,-0.83076923076923,
-0.815384615384614,-0.799999999999999,-0.784615384615384,-0.769230769230768,
-0.753846153846153,-0.738461538461538,-0.723076923076922,-0.707692307692307,
-0.692307692307692,-0.676923076923076,-0.661538461538461,-0.646153846153846,
-0.63076923076923,-0.615384615384615,-0.6,-0.584615384615384,-0.569230769230769,
-0.553846153846154,-0.538461538461538,-0.523076923076923,-0.507692307692308,
-0.492307692307692,-0.476923076923077,-0.461538461538462,-0.446153846153846,
-0.430769230769231,-0.415384615384615,-0.4,-0.384615384615385,-0.369230769230769,
-0.353846153846154,-0.338461538461538,-0.323076923076923,-0.307692307692308,
-0.292307692307692,-0.276923076923077,-0.261538461538462,-0.246153846153846,
-0.230769230769231,-0.215384615384615,-0.2,-0.184615384615385,-0.169230769230769,
-0.153846153846154,-0.138461538461538,-0.123076923076923,-0.107692307692308,
-0.0923076923076923,-0.0769230769230769,-0.0615384615384615,-0.0461538461538462,
-0.0307692307692308,-0.0153846153846154,0.),(-1.,1.),.UNSPECIFIED.)
GEOMETRIC_REPRESENTATION_ITEM()
RATIONAL_B_SPLINE_SURFACE(((1.,1.),(1.,1.),(1.,1.),(1.,1.),(1.,1.),(1.,
1.),(1.,1.),(1.,1.),(1.,1.),(1.,1.),(1.,1.),(1.,1.),(1.,1.),(1.,1.),(1.,
1.),(1.,1.),(1.,1.),(1.,1.),(1.,1.),(1.,1.),(1.,1.),(1.,1.),(1.,1.),(1.,
1.),(1.,1.),(1.,1.),(1.,1.),(1.,1.),(1.,1.),(1.,1.),(1.,1.),(1.,1.),(1.,
1.),(1.,1.),(1.,1.),(1.,1.),(1.,1.),(1.,1.),(1.,1.),(1.,1.),(1.,1.),(1.,
1.),(1.,1.),(1.,1.),(1.,1.),(1.,1.),(1.,1.),(1.,1.),(1.,1.),(1.,1.),(1.,
1.),(1.,1.),(1.,1.),(1.,1.),(1.,1.),(1.,1.),(1.,1.),(1.,1.),(1.,1.),(1.,
1.),(1.,1.),(1.,1.),(1.,1.),(1.,1.),(1.,1.),(1.,1.),(1.,1.),(1.,1.),(1.,
1.),(1.,1.)))
REPRESENTATION_ITEM('')
SURFACE()
);
#38=(
BOUNDED_SURFACE()
B_SPLINE_SURFACE(5,1,((#31612,#31613),(#31614,#31615),(#31616,#31617),(#31618,
#31619),(#31620,#31621),(#31622,#31623),(#31624,#31625),(#31626,#31627),
(#31628,#31629),(#31630,#31631),(#31632,#31633),(#31634,#31635),(#31636,
#31637),(#31638,#31639),(#31640,#31641),(#31642,#31643),(#31644,#31645),
(#31646,#31647),(#31648,#31649),(#31650,#31651),(#31652,#31653),(#31654,
#31655),(#31656,#31657),(#31658,#31659),(#31660,#31661),(#31662,#31663),
(#31664,#31665),(#31666,#31667),(#31668,#31669),(#31670,#31671),(#31672,
#31673),(#31674,#31675),(#31676,#31677),(#31678,#31679),(#31680,#31681),
(#31682,#31683),(#31684,#31685),(#31686,#31687),(#31688,#31689),(#31690,
#31691),(#31692,#31693),(#31694,#31695),(#31696,#31697),(#31698,#31699),
(#31700,#31701),(#31702,#31703),(#31704,#31705),(#31706,#31707),(#31708,
#31709),(#31710,#31711),(#31712,#31713),(#31714,#31715),(#31716,#31717),
(#31718,#31719),(#31720,#31721),(#31722,#31723),(#31724,#31725),(#31726,
#31727),(#31728,#31729),(#31730,#31731),(#31732,#31733),(#31734,#31735),
(#31736,#31737),(#31738,#31739),(#31740,#31741),(#31742,#31743),(#31744,
#31745),(#31746,#31747),(#31748,#31749),(#31750,#31751)),.UNSPECIFIED.,
 .F.,.F.,.F.)
B_SPLINE_SURFACE_WITH_KNOTS((6,1,1,1,1,1,1,1,1,1,1,1,1,1,1,1,1,1,1,1,1,
1,1,1,1,1,1,1,1,1,1,1,1,1,1,1,1,1,1,1,1,1,1,1,1,1,1,1,1,1,1,1,1,1,1,1,1,
1,1,1,1,1,1,1,1,6),(2,2),(-1.,-0.984615384615383,-0.969230769230768,-0.953846153846152,
-0.938461538461537,-0.923076923076922,-0.907692307692306,-0.892307692307691,
-0.876923076923076,-0.86153846153846,-0.846153846153845,-0.83076923076923,
-0.815384615384614,-0.799999999999999,-0.784615384615384,-0.769230769230768,
-0.753846153846153,-0.738461538461538,-0.723076923076922,-0.707692307692307,
-0.692307692307692,-0.676923076923076,-0.661538461538461,-0.646153846153846,
-0.63076923076923,-0.615384615384615,-0.6,-0.584615384615384,-0.569230769230769,
-0.553846153846154,-0.538461538461538,-0.523076923076923,-0.507692307692308,
-0.492307692307692,-0.476923076923077,-0.461538461538462,-0.446153846153846,
-0.430769230769231,-0.415384615384615,-0.4,-0.384615384615385,-0.369230769230769,
-0.353846153846154,-0.338461538461538,-0.323076923076923,-0.307692307692308,
-0.292307692307692,-0.276923076923077,-0.261538461538462,-0.246153846153846,
-0.230769230769231,-0.215384615384615,-0.2,-0.184615384615385,-0.169230769230769,
-0.153846153846154,-0.138461538461538,-0.123076923076923,-0.107692307692308,
-0.0923076923076923,-0.0769230769230769,-0.0615384615384615,-0.0461538461538462,
-0.0307692307692308,-0.0153846153846154,0.),(-1.,1.),.UNSPECIFIED.)
GEOMETRIC_REPRESENTATION_ITEM()
RATIONAL_B_SPLINE_SURFACE(((1.,1.),(1.,1.),(1.,1.),(1.,1.),(1.,1.),(1.,
1.),(1.,1.),(1.,1.),(1.,1.),(1.,1.),(1.,1.),(1.,1.),(1.,1.),(1.,1.),(1.,
1.),(1.,1.),(1.,1.),(1.,1.),(1.,1.),(1.,1.),(1.,1.),(1.,1.),(1.,1.),(1.,
1.),(1.,1.),(1.,1.),(1.,1.),(1.,1.),(1.,1.),(1.,1.),(1.,1.),(1.,1.),(1.,
1.),(1.,1.),(1.,1.),(1.,1.),(1.,1.),(1.,1.),(1.,1.),(1.,1.),(1.,1.),(1.,
1.),(1.,1.),(1.,1.),(1.,1.),(1.,1.),(1.,1.),(1.,1.),(1.,1.),(1.,1.),(1.,
1.),(1.,1.),(1.,1.),(1.,1.),(1.,1.),(1.,1.),(1.,1.),(1.,1.),(1.,1.),(1.,
1.),(1.,1.),(1.,1.),(1.,1.),(1.,1.),(1.,1.),(1.,1.),(1.,1.),(1.,1.),(1.,
1.),(1.,1.)))
REPRESENTATION_ITEM('')
SURFACE()
);
#39=(
BOUNDED_SURFACE()
B_SPLINE_SURFACE(5,1,((#31828,#31829),(#31830,#31831),(#31832,#31833),(#31834,
#31835),(#31836,#31837),(#31838,#31839),(#31840,#31841),(#31842,#31843),
(#31844,#31845),(#31846,#31847),(#31848,#31849),(#31850,#31851),(#31852,
#31853),(#31854,#31855),(#31856,#31857),(#31858,#31859),(#31860,#31861),
(#31862,#31863),(#31864,#31865),(#31866,#31867),(#31868,#31869),(#31870,
#31871),(#31872,#31873),(#31874,#31875),(#31876,#31877),(#31878,#31879),
(#31880,#31881),(#31882,#31883),(#31884,#31885),(#31886,#31887),(#31888,
#31889),(#31890,#31891),(#31892,#31893),(#31894,#31895),(#31896,#31897),
(#31898,#31899),(#31900,#31901),(#31902,#31903),(#31904,#31905),(#31906,
#31907),(#31908,#31909),(#31910,#31911),(#31912,#31913),(#31914,#31915),
(#31916,#31917),(#31918,#31919),(#31920,#31921),(#31922,#31923),(#31924,
#31925),(#31926,#31927),(#31928,#31929),(#31930,#31931),(#31932,#31933),
(#31934,#31935),(#31936,#31937),(#31938,#31939),(#31940,#31941),(#31942,
#31943),(#31944,#31945),(#31946,#31947),(#31948,#31949),(#31950,#31951),
(#31952,#31953),(#31954,#31955),(#31956,#31957),(#31958,#31959),(#31960,
#31961),(#31962,#31963),(#31964,#31965),(#31966,#31967)),.UNSPECIFIED.,
 .F.,.F.,.F.)
B_SPLINE_SURFACE_WITH_KNOTS((6,1,1,1,1,1,1,1,1,1,1,1,1,1,1,1,1,1,1,1,1,
1,1,1,1,1,1,1,1,1,1,1,1,1,1,1,1,1,1,1,1,1,1,1,1,1,1,1,1,1,1,1,1,1,1,1,1,
1,1,1,1,1,1,1,1,6),(2,2),(-1.,-0.984615384615383,-0.969230769230768,-0.953846153846152,
-0.938461538461537,-0.923076923076922,-0.907692307692306,-0.892307692307691,
-0.876923076923076,-0.86153846153846,-0.846153846153845,-0.83076923076923,
-0.815384615384614,-0.799999999999999,-0.784615384615384,-0.769230769230768,
-0.753846153846153,-0.738461538461538,-0.723076923076922,-0.707692307692307,
-0.692307692307692,-0.676923076923076,-0.661538461538461,-0.646153846153846,
-0.63076923076923,-0.615384615384615,-0.6,-0.584615384615384,-0.569230769230769,
-0.553846153846154,-0.538461538461538,-0.523076923076923,-0.507692307692308,
-0.492307692307692,-0.476923076923077,-0.461538461538462,-0.446153846153846,
-0.430769230769231,-0.415384615384615,-0.4,-0.384615384615385,-0.369230769230769,
-0.353846153846154,-0.338461538461538,-0.323076923076923,-0.307692307692308,
-0.292307692307692,-0.276923076923077,-0.261538461538462,-0.246153846153846,
-0.230769230769231,-0.215384615384615,-0.2,-0.184615384615385,-0.169230769230769,
-0.153846153846154,-0.138461538461538,-0.123076923076923,-0.107692307692308,
-0.0923076923076923,-0.0769230769230769,-0.0615384615384615,-0.0461538461538462,
-0.0307692307692308,-0.0153846153846154,0.),(-1.,1.),.UNSPECIFIED.)
GEOMETRIC_REPRESENTATION_ITEM()
RATIONAL_B_SPLINE_SURFACE(((1.,1.),(1.,1.),(1.,1.),(1.,1.),(1.,1.),(1.,
1.),(1.,1.),(1.,1.),(1.,1.),(1.,1.),(1.,1.),(1.,1.),(1.,1.),(1.,1.),(1.,
1.),(1.,1.),(1.,1.),(1.,1.),(1.,1.),(1.,1.),(1.,1.),(1.,1.),(1.,1.),(1.,
1.),(1.,1.),(1.,1.),(1.,1.),(1.,1.),(1.,1.),(1.,1.),(1.,1.),(1.,1.),(1.,
1.),(1.,1.),(1.,1.),(1.,1.),(1.,1.),(1.,1.),(1.,1.),(1.,1.),(1.,1.),(1.,
1.),(1.,1.),(1.,1.),(1.,1.),(1.,1.),(1.,1.),(1.,1.),(1.,1.),(1.,1.),(1.,
1.),(1.,1.),(1.,1.),(1.,1.),(1.,1.),(1.,1.),(1.,1.),(1.,1.),(1.,1.),(1.,
1.),(1.,1.),(1.,1.),(1.,1.),(1.,1.),(1.,1.),(1.,1.),(1.,1.),(1.,1.),(1.,
1.),(1.,1.)))
REPRESENTATION_ITEM('')
SURFACE()
);
#40=(
BOUNDED_SURFACE()
B_SPLINE_SURFACE(5,1,((#32044,#32045),(#32046,#32047),(#32048,#32049),(#32050,
#32051),(#32052,#32053),(#32054,#32055),(#32056,#32057),(#32058,#32059),
(#32060,#32061),(#32062,#32063),(#32064,#32065),(#32066,#32067),(#32068,
#32069),(#32070,#32071),(#32072,#32073),(#32074,#32075),(#32076,#32077),
(#32078,#32079),(#32080,#32081),(#32082,#32083),(#32084,#32085),(#32086,
#32087),(#32088,#32089),(#32090,#32091),(#32092,#32093),(#32094,#32095),
(#32096,#32097),(#32098,#32099),(#32100,#32101),(#32102,#32103),(#32104,
#32105),(#32106,#32107),(#32108,#32109),(#32110,#32111),(#32112,#32113),
(#32114,#32115),(#32116,#32117),(#32118,#32119),(#32120,#32121),(#32122,
#32123),(#32124,#32125),(#32126,#32127),(#32128,#32129),(#32130,#32131),
(#32132,#32133),(#32134,#32135),(#32136,#32137),(#32138,#32139),(#32140,
#32141),(#32142,#32143),(#32144,#32145),(#32146,#32147),(#32148,#32149),
(#32150,#32151),(#32152,#32153),(#32154,#32155),(#32156,#32157),(#32158,
#32159),(#32160,#32161),(#32162,#32163),(#32164,#32165),(#32166,#32167),
(#32168,#32169),(#32170,#32171),(#32172,#32173),(#32174,#32175),(#32176,
#32177),(#32178,#32179),(#32180,#32181),(#32182,#32183)),.UNSPECIFIED.,
 .F.,.F.,.F.)
B_SPLINE_SURFACE_WITH_KNOTS((6,1,1,1,1,1,1,1,1,1,1,1,1,1,1,1,1,1,1,1,1,
1,1,1,1,1,1,1,1,1,1,1,1,1,1,1,1,1,1,1,1,1,1,1,1,1,1,1,1,1,1,1,1,1,1,1,1,
1,1,1,1,1,1,1,1,6),(2,2),(-1.,-0.984615384615383,-0.969230769230768,-0.953846153846152,
-0.938461538461537,-0.923076923076922,-0.907692307692306,-0.892307692307691,
-0.876923076923076,-0.86153846153846,-0.846153846153845,-0.83076923076923,
-0.815384615384614,-0.799999999999999,-0.784615384615384,-0.769230769230768,
-0.753846153846153,-0.738461538461538,-0.723076923076922,-0.707692307692307,
-0.692307692307692,-0.676923076923076,-0.661538461538461,-0.646153846153846,
-0.63076923076923,-0.615384615384615,-0.6,-0.584615384615384,-0.569230769230769,
-0.553846153846154,-0.538461538461538,-0.523076923076923,-0.507692307692308,
-0.492307692307692,-0.476923076923077,-0.461538461538462,-0.446153846153846,
-0.430769230769231,-0.415384615384615,-0.4,-0.384615384615385,-0.369230769230769,
-0.353846153846154,-0.338461538461538,-0.323076923076923,-0.307692307692308,
-0.292307692307692,-0.276923076923077,-0.261538461538462,-0.246153846153846,
-0.230769230769231,-0.215384615384615,-0.2,-0.184615384615385,-0.169230769230769,
-0.153846153846154,-0.138461538461538,-0.123076923076923,-0.107692307692308,
-0.0923076923076923,-0.0769230769230769,-0.0615384615384615,-0.0461538461538462,
-0.0307692307692308,-0.0153846153846154,0.),(-1.,1.),.UNSPECIFIED.)
GEOMETRIC_REPRESENTATION_ITEM()
RATIONAL_B_SPLINE_SURFACE(((1.,1.),(1.,1.),(1.,1.),(1.,1.),(1.,1.),(1.,
1.),(1.,1.),(1.,1.),(1.,1.),(1.,1.),(1.,1.),(1.,1.),(1.,1.),(1.,1.),(1.,
1.),(1.,1.),(1.,1.),(1.,1.),(1.,1.),(1.,1.),(1.,1.),(1.,1.),(1.,1.),(1.,
1.),(1.,1.),(1.,1.),(1.,1.),(1.,1.),(1.,1.),(1.,1.),(1.,1.),(1.,1.),(1.,
1.),(1.,1.),(1.,1.),(1.,1.),(1.,1.),(1.,1.),(1.,1.),(1.,1.),(1.,1.),(1.,
1.),(1.,1.),(1.,1.),(1.,1.),(1.,1.),(1.,1.),(1.,1.),(1.,1.),(1.,1.),(1.,
1.),(1.,1.),(1.,1.),(1.,1.),(1.,1.),(1.,1.),(1.,1.),(1.,1.),(1.,1.),(1.,
1.),(1.,1.),(1.,1.),(1.,1.),(1.,1.),(1.,1.),(1.,1.),(1.,1.),(1.,1.),(1.,
1.),(1.,1.)))
REPRESENTATION_ITEM('')
SURFACE()
);
#41=(
BOUNDED_SURFACE()
B_SPLINE_SURFACE(5,1,((#32260,#32261),(#32262,#32263),(#32264,#32265),(#32266,
#32267),(#32268,#32269),(#32270,#32271),(#32272,#32273),(#32274,#32275),
(#32276,#32277),(#32278,#32279),(#32280,#32281),(#32282,#32283),(#32284,
#32285),(#32286,#32287),(#32288,#32289),(#32290,#32291),(#32292,#32293),
(#32294,#32295),(#32296,#32297),(#32298,#32299),(#32300,#32301),(#32302,
#32303),(#32304,#32305),(#32306,#32307),(#32308,#32309),(#32310,#32311),
(#32312,#32313),(#32314,#32315),(#32316,#32317),(#32318,#32319),(#32320,
#32321),(#32322,#32323),(#32324,#32325),(#32326,#32327),(#32328,#32329),
(#32330,#32331),(#32332,#32333),(#32334,#32335),(#32336,#32337),(#32338,
#32339),(#32340,#32341),(#32342,#32343),(#32344,#32345),(#32346,#32347),
(#32348,#32349),(#32350,#32351),(#32352,#32353),(#32354,#32355),(#32356,
#32357),(#32358,#32359),(#32360,#32361),(#32362,#32363),(#32364,#32365),
(#32366,#32367),(#32368,#32369),(#32370,#32371),(#32372,#32373),(#32374,
#32375),(#32376,#32377),(#32378,#32379),(#32380,#32381),(#32382,#32383),
(#32384,#32385),(#32386,#32387),(#32388,#32389),(#32390,#32391),(#32392,
#32393),(#32394,#32395),(#32396,#32397),(#32398,#32399)),.UNSPECIFIED.,
 .F.,.F.,.F.)
B_SPLINE_SURFACE_WITH_KNOTS((6,1,1,1,1,1,1,1,1,1,1,1,1,1,1,1,1,1,1,1,1,
1,1,1,1,1,1,1,1,1,1,1,1,1,1,1,1,1,1,1,1,1,1,1,1,1,1,1,1,1,1,1,1,1,1,1,1,
1,1,1,1,1,1,1,1,6),(2,2),(-1.,-0.984615384615383,-0.969230769230768,-0.953846153846152,
-0.938461538461537,-0.923076923076922,-0.907692307692306,-0.892307692307691,
-0.876923076923076,-0.86153846153846,-0.846153846153845,-0.83076923076923,
-0.815384615384614,-0.799999999999999,-0.784615384615384,-0.769230769230768,
-0.753846153846153,-0.738461538461538,-0.723076923076922,-0.707692307692307,
-0.692307692307692,-0.676923076923076,-0.661538461538461,-0.646153846153846,
-0.63076923076923,-0.615384615384615,-0.6,-0.584615384615384,-0.569230769230769,
-0.553846153846154,-0.538461538461538,-0.523076923076923,-0.507692307692308,
-0.492307692307692,-0.476923076923077,-0.461538461538462,-0.446153846153846,
-0.430769230769231,-0.415384615384615,-0.4,-0.384615384615385,-0.369230769230769,
-0.353846153846154,-0.338461538461538,-0.323076923076923,-0.307692307692308,
-0.292307692307692,-0.276923076923077,-0.261538461538462,-0.246153846153846,
-0.230769230769231,-0.215384615384615,-0.2,-0.184615384615385,-0.169230769230769,
-0.153846153846154,-0.138461538461538,-0.123076923076923,-0.107692307692308,
-0.0923076923076923,-0.0769230769230769,-0.0615384615384615,-0.0461538461538462,
-0.0307692307692308,-0.0153846153846154,0.),(-1.,1.),.UNSPECIFIED.)
GEOMETRIC_REPRESENTATION_ITEM()
RATIONAL_B_SPLINE_SURFACE(((1.,1.),(1.,1.),(1.,1.),(1.,1.),(1.,1.),(1.,
1.),(1.,1.),(1.,1.),(1.,1.),(1.,1.),(1.,1.),(1.,1.),(1.,1.),(1.,1.),(1.,
1.),(1.,1.),(1.,1.),(1.,1.),(1.,1.),(1.,1.),(1.,1.),(1.,1.),(1.,1.),(1.,
1.),(1.,1.),(1.,1.),(1.,1.),(1.,1.),(1.,1.),(1.,1.),(1.,1.),(1.,1.),(1.,
1.),(1.,1.),(1.,1.),(1.,1.),(1.,1.),(1.,1.),(1.,1.),(1.,1.),(1.,1.),(1.,
1.),(1.,1.),(1.,1.),(1.,1.),(1.,1.),(1.,1.),(1.,1.),(1.,1.),(1.,1.),(1.,
1.),(1.,1.),(1.,1.),(1.,1.),(1.,1.),(1.,1.),(1.,1.),(1.,1.),(1.,1.),(1.,
1.),(1.,1.),(1.,1.),(1.,1.),(1.,1.),(1.,1.),(1.,1.),(1.,1.),(1.,1.),(1.,
1.),(1.,1.)))
REPRESENTATION_ITEM('')
SURFACE()
);
#42=(
BOUNDED_SURFACE()
B_SPLINE_SURFACE(5,1,((#32476,#32477),(#32478,#32479),(#32480,#32481),(#32482,
#32483),(#32484,#32485),(#32486,#32487),(#32488,#32489),(#32490,#32491),
(#32492,#32493),(#32494,#32495),(#32496,#32497),(#32498,#32499),(#32500,
#32501),(#32502,#32503),(#32504,#32505),(#32506,#32507),(#32508,#32509),
(#32510,#32511),(#32512,#32513),(#32514,#32515),(#32516,#32517),(#32518,
#32519),(#32520,#32521),(#32522,#32523),(#32524,#32525),(#32526,#32527),
(#32528,#32529),(#32530,#32531),(#32532,#32533),(#32534,#32535),(#32536,
#32537),(#32538,#32539),(#32540,#32541),(#32542,#32543),(#32544,#32545),
(#32546,#32547),(#32548,#32549),(#32550,#32551),(#32552,#32553),(#32554,
#32555),(#32556,#32557),(#32558,#32559),(#32560,#32561),(#32562,#32563),
(#32564,#32565),(#32566,#32567),(#32568,#32569),(#32570,#32571),(#32572,
#32573),(#32574,#32575),(#32576,#32577),(#32578,#32579),(#32580,#32581),
(#32582,#32583),(#32584,#32585),(#32586,#32587),(#32588,#32589),(#32590,
#32591),(#32592,#32593),(#32594,#32595),(#32596,#32597),(#32598,#32599),
(#32600,#32601),(#32602,#32603),(#32604,#32605),(#32606,#32607),(#32608,
#32609),(#32610,#32611),(#32612,#32613),(#32614,#32615)),.UNSPECIFIED.,
 .F.,.F.,.F.)
B_SPLINE_SURFACE_WITH_KNOTS((6,1,1,1,1,1,1,1,1,1,1,1,1,1,1,1,1,1,1,1,1,
1,1,1,1,1,1,1,1,1,1,1,1,1,1,1,1,1,1,1,1,1,1,1,1,1,1,1,1,1,1,1,1,1,1,1,1,
1,1,1,1,1,1,1,1,6),(2,2),(-1.,-0.984615384615383,-0.969230769230768,-0.953846153846152,
-0.938461538461537,-0.923076923076922,-0.907692307692306,-0.892307692307691,
-0.876923076923076,-0.86153846153846,-0.846153846153845,-0.83076923076923,
-0.815384615384614,-0.799999999999999,-0.784615384615384,-0.769230769230768,
-0.753846153846153,-0.738461538461538,-0.723076923076922,-0.707692307692307,
-0.692307692307692,-0.676923076923076,-0.661538461538461,-0.646153846153846,
-0.63076923076923,-0.615384615384615,-0.6,-0.584615384615384,-0.569230769230769,
-0.553846153846154,-0.538461538461538,-0.523076923076923,-0.507692307692308,
-0.492307692307692,-0.476923076923077,-0.461538461538462,-0.446153846153846,
-0.430769230769231,-0.415384615384615,-0.4,-0.384615384615385,-0.369230769230769,
-0.353846153846154,-0.338461538461538,-0.323076923076923,-0.307692307692308,
-0.292307692307692,-0.276923076923077,-0.261538461538462,-0.246153846153846,
-0.230769230769231,-0.215384615384615,-0.2,-0.184615384615385,-0.169230769230769,
-0.153846153846154,-0.138461538461538,-0.123076923076923,-0.107692307692308,
-0.0923076923076923,-0.0769230769230769,-0.0615384615384615,-0.0461538461538462,
-0.0307692307692308,-0.0153846153846154,0.),(-1.,1.),.UNSPECIFIED.)
GEOMETRIC_REPRESENTATION_ITEM()
RATIONAL_B_SPLINE_SURFACE(((1.,1.),(1.,1.),(1.,1.),(1.,1.),(1.,1.),(1.,
1.),(1.,1.),(1.,1.),(1.,1.),(1.,1.),(1.,1.),(1.,1.),(1.,1.),(1.,1.),(1.,
1.),(1.,1.),(1.,1.),(1.,1.),(1.,1.),(1.,1.),(1.,1.),(1.,1.),(1.,1.),(1.,
1.),(1.,1.),(1.,1.),(1.,1.),(1.,1.),(1.,1.),(1.,1.),(1.,1.),(1.,1.),(1.,
1.),(1.,1.),(1.,1.),(1.,1.),(1.,1.),(1.,1.),(1.,1.),(1.,1.),(1.,1.),(1.,
1.),(1.,1.),(1.,1.),(1.,1.),(1.,1.),(1.,1.),(1.,1.),(1.,1.),(1.,1.),(1.,
1.),(1.,1.),(1.,1.),(1.,1.),(1.,1.),(1.,1.),(1.,1.),(1.,1.),(1.,1.),(1.,
1.),(1.,1.),(1.,1.),(1.,1.),(1.,1.),(1.,1.),(1.,1.),(1.,1.),(1.,1.),(1.,
1.),(1.,1.)))
REPRESENTATION_ITEM('')
SURFACE()
);
#43=(
BOUNDED_SURFACE()
B_SPLINE_SURFACE(5,1,((#32692,#32693),(#32694,#32695),(#32696,#32697),(#32698,
#32699),(#32700,#32701),(#32702,#32703),(#32704,#32705),(#32706,#32707),
(#32708,#32709),(#32710,#32711),(#32712,#32713),(#32714,#32715),(#32716,
#32717),(#32718,#32719),(#32720,#32721),(#32722,#32723),(#32724,#32725),
(#32726,#32727),(#32728,#32729),(#32730,#32731),(#32732,#32733),(#32734,
#32735),(#32736,#32737),(#32738,#32739),(#32740,#32741),(#32742,#32743),
(#32744,#32745),(#32746,#32747),(#32748,#32749),(#32750,#32751),(#32752,
#32753),(#32754,#32755),(#32756,#32757),(#32758,#32759),(#32760,#32761),
(#32762,#32763),(#32764,#32765),(#32766,#32767),(#32768,#32769),(#32770,
#32771),(#32772,#32773),(#32774,#32775),(#32776,#32777),(#32778,#32779),
(#32780,#32781),(#32782,#32783),(#32784,#32785),(#32786,#32787),(#32788,
#32789),(#32790,#32791),(#32792,#32793),(#32794,#32795),(#32796,#32797),
(#32798,#32799),(#32800,#32801),(#32802,#32803),(#32804,#32805),(#32806,
#32807),(#32808,#32809),(#32810,#32811),(#32812,#32813),(#32814,#32815),
(#32816,#32817),(#32818,#32819),(#32820,#32821),(#32822,#32823),(#32824,
#32825),(#32826,#32827),(#32828,#32829),(#32830,#32831)),.UNSPECIFIED.,
 .F.,.F.,.F.)
B_SPLINE_SURFACE_WITH_KNOTS((6,1,1,1,1,1,1,1,1,1,1,1,1,1,1,1,1,1,1,1,1,
1,1,1,1,1,1,1,1,1,1,1,1,1,1,1,1,1,1,1,1,1,1,1,1,1,1,1,1,1,1,1,1,1,1,1,1,
1,1,1,1,1,1,1,1,6),(2,2),(-1.,-0.984615384615383,-0.969230769230768,-0.953846153846152,
-0.938461538461537,-0.923076923076922,-0.907692307692306,-0.892307692307691,
-0.876923076923076,-0.86153846153846,-0.846153846153845,-0.83076923076923,
-0.815384615384614,-0.799999999999999,-0.784615384615384,-0.769230769230768,
-0.753846153846153,-0.738461538461538,-0.723076923076922,-0.707692307692307,
-0.692307692307692,-0.676923076923076,-0.661538461538461,-0.646153846153846,
-0.63076923076923,-0.615384615384615,-0.6,-0.584615384615384,-0.569230769230769,
-0.553846153846154,-0.538461538461538,-0.523076923076923,-0.507692307692308,
-0.492307692307692,-0.476923076923077,-0.461538461538462,-0.446153846153846,
-0.430769230769231,-0.415384615384615,-0.4,-0.384615384615385,-0.369230769230769,
-0.353846153846154,-0.338461538461538,-0.323076923076923,-0.307692307692308,
-0.292307692307692,-0.276923076923077,-0.261538461538462,-0.246153846153846,
-0.230769230769231,-0.215384615384615,-0.2,-0.184615384615385,-0.169230769230769,
-0.153846153846154,-0.138461538461538,-0.123076923076923,-0.107692307692308,
-0.0923076923076923,-0.0769230769230769,-0.0615384615384615,-0.0461538461538462,
-0.0307692307692308,-0.0153846153846154,0.),(-1.,1.),.UNSPECIFIED.)
GEOMETRIC_REPRESENTATION_ITEM()
RATIONAL_B_SPLINE_SURFACE(((1.,1.),(1.,1.),(1.,1.),(1.,1.),(1.,1.),(1.,
1.),(1.,1.),(1.,1.),(1.,1.),(1.,1.),(1.,1.),(1.,1.),(1.,1.),(1.,1.),(1.,
1.),(1.,1.),(1.,1.),(1.,1.),(1.,1.),(1.,1.),(1.,1.),(1.,1.),(1.,1.),(1.,
1.),(1.,1.),(1.,1.),(1.,1.),(1.,1.),(1.,1.),(1.,1.),(1.,1.),(1.,1.),(1.,
1.),(1.,1.),(1.,1.),(1.,1.),(1.,1.),(1.,1.),(1.,1.),(1.,1.),(1.,1.),(1.,
1.),(1.,1.),(1.,1.),(1.,1.),(1.,1.),(1.,1.),(1.,1.),(1.,1.),(1.,1.),(1.,
1.),(1.,1.),(1.,1.),(1.,1.),(1.,1.),(1.,1.),(1.,1.),(1.,1.),(1.,1.),(1.,
1.),(1.,1.),(1.,1.),(1.,1.),(1.,1.),(1.,1.),(1.,1.),(1.,1.),(1.,1.),(1.,
1.),(1.,1.)))
REPRESENTATION_ITEM('')
SURFACE()
);
#44=(
BOUNDED_SURFACE()
B_SPLINE_SURFACE(5,1,((#32908,#32909),(#32910,#32911),(#32912,#32913),(#32914,
#32915),(#32916,#32917),(#32918,#32919),(#32920,#32921),(#32922,#32923),
(#32924,#32925),(#32926,#32927),(#32928,#32929),(#32930,#32931),(#32932,
#32933),(#32934,#32935),(#32936,#32937),(#32938,#32939),(#32940,#32941),
(#32942,#32943),(#32944,#32945),(#32946,#32947),(#32948,#32949),(#32950,
#32951),(#32952,#32953),(#32954,#32955),(#32956,#32957),(#32958,#32959),
(#32960,#32961),(#32962,#32963),(#32964,#32965),(#32966,#32967),(#32968,
#32969),(#32970,#32971),(#32972,#32973),(#32974,#32975),(#32976,#32977),
(#32978,#32979),(#32980,#32981),(#32982,#32983),(#32984,#32985),(#32986,
#32987),(#32988,#32989),(#32990,#32991),(#32992,#32993),(#32994,#32995),
(#32996,#32997),(#32998,#32999),(#33000,#33001),(#33002,#33003),(#33004,
#33005),(#33006,#33007),(#33008,#33009),(#33010,#33011),(#33012,#33013),
(#33014,#33015),(#33016,#33017),(#33018,#33019),(#33020,#33021),(#33022,
#33023),(#33024,#33025),(#33026,#33027),(#33028,#33029),(#33030,#33031),
(#33032,#33033),(#33034,#33035),(#33036,#33037),(#33038,#33039),(#33040,
#33041),(#33042,#33043),(#33044,#33045),(#33046,#33047)),.UNSPECIFIED.,
 .F.,.F.,.F.)
B_SPLINE_SURFACE_WITH_KNOTS((6,1,1,1,1,1,1,1,1,1,1,1,1,1,1,1,1,1,1,1,1,
1,1,1,1,1,1,1,1,1,1,1,1,1,1,1,1,1,1,1,1,1,1,1,1,1,1,1,1,1,1,1,1,1,1,1,1,
1,1,1,1,1,1,1,1,6),(2,2),(-1.,-0.984615384615383,-0.969230769230768,-0.953846153846152,
-0.938461538461537,-0.923076923076922,-0.907692307692306,-0.892307692307691,
-0.876923076923076,-0.86153846153846,-0.846153846153845,-0.83076923076923,
-0.815384615384614,-0.799999999999999,-0.784615384615384,-0.769230769230768,
-0.753846153846153,-0.738461538461538,-0.723076923076922,-0.707692307692307,
-0.692307692307692,-0.676923076923076,-0.661538461538461,-0.646153846153846,
-0.63076923076923,-0.615384615384615,-0.6,-0.584615384615384,-0.569230769230769,
-0.553846153846154,-0.538461538461538,-0.523076923076923,-0.507692307692308,
-0.492307692307692,-0.476923076923077,-0.461538461538462,-0.446153846153846,
-0.430769230769231,-0.415384615384615,-0.4,-0.384615384615385,-0.369230769230769,
-0.353846153846154,-0.338461538461538,-0.323076923076923,-0.307692307692308,
-0.292307692307692,-0.276923076923077,-0.261538461538462,-0.246153846153846,
-0.230769230769231,-0.215384615384615,-0.2,-0.184615384615385,-0.169230769230769,
-0.153846153846154,-0.138461538461538,-0.123076923076923,-0.107692307692308,
-0.0923076923076923,-0.0769230769230769,-0.0615384615384615,-0.0461538461538462,
-0.0307692307692308,-0.0153846153846154,0.),(-1.,1.),.UNSPECIFIED.)
GEOMETRIC_REPRESENTATION_ITEM()
RATIONAL_B_SPLINE_SURFACE(((1.,1.),(1.,1.),(1.,1.),(1.,1.),(1.,1.),(1.,
1.),(1.,1.),(1.,1.),(1.,1.),(1.,1.),(1.,1.),(1.,1.),(1.,1.),(1.,1.),(1.,
1.),(1.,1.),(1.,1.),(1.,1.),(1.,1.),(1.,1.),(1.,1.),(1.,1.),(1.,1.),(1.,
1.),(1.,1.),(1.,1.),(1.,1.),(1.,1.),(1.,1.),(1.,1.),(1.,1.),(1.,1.),(1.,
1.),(1.,1.),(1.,1.),(1.,1.),(1.,1.),(1.,1.),(1.,1.),(1.,1.),(1.,1.),(1.,
1.),(1.,1.),(1.,1.),(1.,1.),(1.,1.),(1.,1.),(1.,1.),(1.,1.),(1.,1.),(1.,
1.),(1.,1.),(1.,1.),(1.,1.),(1.,1.),(1.,1.),(1.,1.),(1.,1.),(1.,1.),(1.,
1.),(1.,1.),(1.,1.),(1.,1.),(1.,1.),(1.,1.),(1.,1.),(1.,1.),(1.,1.),(1.,
1.),(1.,1.)))
REPRESENTATION_ITEM('')
SURFACE()
);
#45=(
BOUNDED_SURFACE()
B_SPLINE_SURFACE(5,1,((#33124,#33125),(#33126,#33127),(#33128,#33129),(#33130,
#33131),(#33132,#33133),(#33134,#33135),(#33136,#33137),(#33138,#33139),
(#33140,#33141),(#33142,#33143),(#33144,#33145),(#33146,#33147),(#33148,
#33149),(#33150,#33151),(#33152,#33153),(#33154,#33155),(#33156,#33157),
(#33158,#33159),(#33160,#33161),(#33162,#33163),(#33164,#33165),(#33166,
#33167),(#33168,#33169),(#33170,#33171),(#33172,#33173),(#33174,#33175),
(#33176,#33177),(#33178,#33179),(#33180,#33181),(#33182,#33183),(#33184,
#33185),(#33186,#33187),(#33188,#33189),(#33190,#33191),(#33192,#33193),
(#33194,#33195),(#33196,#33197),(#33198,#33199),(#33200,#33201),(#33202,
#33203),(#33204,#33205),(#33206,#33207),(#33208,#33209),(#33210,#33211),
(#33212,#33213),(#33214,#33215),(#33216,#33217),(#33218,#33219),(#33220,
#33221),(#33222,#33223),(#33224,#33225),(#33226,#33227),(#33228,#33229),
(#33230,#33231),(#33232,#33233),(#33234,#33235),(#33236,#33237),(#33238,
#33239),(#33240,#33241),(#33242,#33243),(#33244,#33245),(#33246,#33247),
(#33248,#33249),(#33250,#33251),(#33252,#33253),(#33254,#33255),(#33256,
#33257),(#33258,#33259),(#33260,#33261),(#33262,#33263)),.UNSPECIFIED.,
 .F.,.F.,.F.)
B_SPLINE_SURFACE_WITH_KNOTS((6,1,1,1,1,1,1,1,1,1,1,1,1,1,1,1,1,1,1,1,1,
1,1,1,1,1,1,1,1,1,1,1,1,1,1,1,1,1,1,1,1,1,1,1,1,1,1,1,1,1,1,1,1,1,1,1,1,
1,1,1,1,1,1,1,1,6),(2,2),(-1.,-0.984615384615383,-0.969230769230768,-0.953846153846152,
-0.938461538461537,-0.923076923076922,-0.907692307692306,-0.892307692307691,
-0.876923076923076,-0.86153846153846,-0.846153846153845,-0.83076923076923,
-0.815384615384614,-0.799999999999999,-0.784615384615384,-0.769230769230768,
-0.753846153846153,-0.738461538461538,-0.723076923076922,-0.707692307692307,
-0.692307692307692,-0.676923076923076,-0.661538461538461,-0.646153846153846,
-0.63076923076923,-0.615384615384615,-0.6,-0.584615384615384,-0.569230769230769,
-0.553846153846154,-0.538461538461538,-0.523076923076923,-0.507692307692308,
-0.492307692307692,-0.476923076923077,-0.461538461538462,-0.446153846153846,
-0.430769230769231,-0.415384615384615,-0.4,-0.384615384615385,-0.369230769230769,
-0.353846153846154,-0.338461538461538,-0.323076923076923,-0.307692307692308,
-0.292307692307692,-0.276923076923077,-0.261538461538462,-0.246153846153846,
-0.230769230769231,-0.215384615384615,-0.2,-0.184615384615385,-0.169230769230769,
-0.153846153846154,-0.138461538461538,-0.123076923076923,-0.107692307692308,
-0.0923076923076923,-0.0769230769230769,-0.0615384615384615,-0.0461538461538462,
-0.0307692307692308,-0.0153846153846154,0.),(-1.,1.),.UNSPECIFIED.)
GEOMETRIC_REPRESENTATION_ITEM()
RATIONAL_B_SPLINE_SURFACE(((1.,1.),(1.,1.),(1.,1.),(1.,1.),(1.,1.),(1.,
1.),(1.,1.),(1.,1.),(1.,1.),(1.,1.),(1.,1.),(1.,1.),(1.,1.),(1.,1.),(1.,
1.),(1.,1.),(1.,1.),(1.,1.),(1.,1.),(1.,1.),(1.,1.),(1.,1.),(1.,1.),(1.,
1.),(1.,1.),(1.,1.),(1.,1.),(1.,1.),(1.,1.),(1.,1.),(1.,1.),(1.,1.),(1.,
1.),(1.,1.),(1.,1.),(1.,1.),(1.,1.),(1.,1.),(1.,1.),(1.,1.),(1.,1.),(1.,
1.),(1.,1.),(1.,1.),(1.,1.),(1.,1.),(1.,1.),(1.,1.),(1.,1.),(1.,1.),(1.,
1.),(1.,1.),(1.,1.),(1.,1.),(1.,1.),(1.,1.),(1.,1.),(1.,1.),(1.,1.),(1.,
1.),(1.,1.),(1.,1.),(1.,1.),(1.,1.),(1.,1.),(1.,1.),(1.,1.),(1.,1.),(1.,
1.),(1.,1.)))
REPRESENTATION_ITEM('')
SURFACE()
);
#46=(
BOUNDED_SURFACE()
B_SPLINE_SURFACE(5,1,((#33340,#33341),(#33342,#33343),(#33344,#33345),(#33346,
#33347),(#33348,#33349),(#33350,#33351),(#33352,#33353),(#33354,#33355),
(#33356,#33357),(#33358,#33359),(#33360,#33361),(#33362,#33363),(#33364,
#33365),(#33366,#33367),(#33368,#33369),(#33370,#33371),(#33372,#33373),
(#33374,#33375),(#33376,#33377),(#33378,#33379),(#33380,#33381),(#33382,
#33383),(#33384,#33385),(#33386,#33387),(#33388,#33389),(#33390,#33391),
(#33392,#33393),(#33394,#33395),(#33396,#33397),(#33398,#33399),(#33400,
#33401),(#33402,#33403),(#33404,#33405),(#33406,#33407),(#33408,#33409),
(#33410,#33411),(#33412,#33413),(#33414,#33415),(#33416,#33417),(#33418,
#33419),(#33420,#33421),(#33422,#33423),(#33424,#33425),(#33426,#33427),
(#33428,#33429),(#33430,#33431),(#33432,#33433),(#33434,#33435),(#33436,
#33437),(#33438,#33439),(#33440,#33441),(#33442,#33443),(#33444,#33445),
(#33446,#33447),(#33448,#33449),(#33450,#33451),(#33452,#33453),(#33454,
#33455),(#33456,#33457),(#33458,#33459),(#33460,#33461),(#33462,#33463),
(#33464,#33465),(#33466,#33467),(#33468,#33469),(#33470,#33471),(#33472,
#33473),(#33474,#33475),(#33476,#33477),(#33478,#33479)),.UNSPECIFIED.,
 .F.,.F.,.F.)
B_SPLINE_SURFACE_WITH_KNOTS((6,1,1,1,1,1,1,1,1,1,1,1,1,1,1,1,1,1,1,1,1,
1,1,1,1,1,1,1,1,1,1,1,1,1,1,1,1,1,1,1,1,1,1,1,1,1,1,1,1,1,1,1,1,1,1,1,1,
1,1,1,1,1,1,1,1,6),(2,2),(-1.,-0.984615384615383,-0.969230769230768,-0.953846153846152,
-0.938461538461537,-0.923076923076922,-0.907692307692306,-0.892307692307691,
-0.876923076923076,-0.86153846153846,-0.846153846153845,-0.83076923076923,
-0.815384615384614,-0.799999999999999,-0.784615384615384,-0.769230769230768,
-0.753846153846153,-0.738461538461538,-0.723076923076922,-0.707692307692307,
-0.692307692307692,-0.676923076923076,-0.661538461538461,-0.646153846153846,
-0.63076923076923,-0.615384615384615,-0.6,-0.584615384615384,-0.569230769230769,
-0.553846153846154,-0.538461538461538,-0.523076923076923,-0.507692307692308,
-0.492307692307692,-0.476923076923077,-0.461538461538462,-0.446153846153846,
-0.430769230769231,-0.415384615384615,-0.4,-0.384615384615385,-0.369230769230769,
-0.353846153846154,-0.338461538461538,-0.323076923076923,-0.307692307692308,
-0.292307692307692,-0.276923076923077,-0.261538461538462,-0.246153846153846,
-0.230769230769231,-0.215384615384615,-0.2,-0.184615384615385,-0.169230769230769,
-0.153846153846154,-0.138461538461538,-0.123076923076923,-0.107692307692308,
-0.0923076923076923,-0.0769230769230769,-0.0615384615384615,-0.0461538461538462,
-0.0307692307692308,-0.0153846153846154,0.),(-1.,1.),.UNSPECIFIED.)
GEOMETRIC_REPRESENTATION_ITEM()
RATIONAL_B_SPLINE_SURFACE(((1.,1.),(1.,1.),(1.,1.),(1.,1.),(1.,1.),(1.,
1.),(1.,1.),(1.,1.),(1.,1.),(1.,1.),(1.,1.),(1.,1.),(1.,1.),(1.,1.),(1.,
1.),(1.,1.),(1.,1.),(1.,1.),(1.,1.),(1.,1.),(1.,1.),(1.,1.),(1.,1.),(1.,
1.),(1.,1.),(1.,1.),(1.,1.),(1.,1.),(1.,1.),(1.,1.),(1.,1.),(1.,1.),(1.,
1.),(1.,1.),(1.,1.),(1.,1.),(1.,1.),(1.,1.),(1.,1.),(1.,1.),(1.,1.),(1.,
1.),(1.,1.),(1.,1.),(1.,1.),(1.,1.),(1.,1.),(1.,1.),(1.,1.),(1.,1.),(1.,
1.),(1.,1.),(1.,1.),(1.,1.),(1.,1.),(1.,1.),(1.,1.),(1.,1.),(1.,1.),(1.,
1.),(1.,1.),(1.,1.),(1.,1.),(1.,1.),(1.,1.),(1.,1.),(1.,1.),(1.,1.),(1.,
1.),(1.,1.)))
REPRESENTATION_ITEM('')
SURFACE()
);
#47=(
BOUNDED_SURFACE()
B_SPLINE_SURFACE(5,1,((#33556,#33557),(#33558,#33559),(#33560,#33561),(#33562,
#33563),(#33564,#33565),(#33566,#33567),(#33568,#33569),(#33570,#33571),
(#33572,#33573),(#33574,#33575),(#33576,#33577),(#33578,#33579),(#33580,
#33581),(#33582,#33583),(#33584,#33585),(#33586,#33587),(#33588,#33589),
(#33590,#33591),(#33592,#33593),(#33594,#33595),(#33596,#33597),(#33598,
#33599),(#33600,#33601),(#33602,#33603),(#33604,#33605),(#33606,#33607),
(#33608,#33609),(#33610,#33611),(#33612,#33613),(#33614,#33615),(#33616,
#33617),(#33618,#33619),(#33620,#33621),(#33622,#33623),(#33624,#33625),
(#33626,#33627),(#33628,#33629),(#33630,#33631),(#33632,#33633),(#33634,
#33635),(#33636,#33637),(#33638,#33639),(#33640,#33641),(#33642,#33643),
(#33644,#33645),(#33646,#33647),(#33648,#33649),(#33650,#33651),(#33652,
#33653),(#33654,#33655),(#33656,#33657),(#33658,#33659),(#33660,#33661),
(#33662,#33663),(#33664,#33665),(#33666,#33667),(#33668,#33669),(#33670,
#33671),(#33672,#33673),(#33674,#33675),(#33676,#33677),(#33678,#33679),
(#33680,#33681),(#33682,#33683),(#33684,#33685),(#33686,#33687),(#33688,
#33689),(#33690,#33691),(#33692,#33693),(#33694,#33695)),.UNSPECIFIED.,
 .F.,.F.,.F.)
B_SPLINE_SURFACE_WITH_KNOTS((6,1,1,1,1,1,1,1,1,1,1,1,1,1,1,1,1,1,1,1,1,
1,1,1,1,1,1,1,1,1,1,1,1,1,1,1,1,1,1,1,1,1,1,1,1,1,1,1,1,1,1,1,1,1,1,1,1,
1,1,1,1,1,1,1,1,6),(2,2),(-1.,-0.984615384615383,-0.969230769230768,-0.953846153846152,
-0.938461538461537,-0.923076923076922,-0.907692307692306,-0.892307692307691,
-0.876923076923076,-0.86153846153846,-0.846153846153845,-0.83076923076923,
-0.815384615384614,-0.799999999999999,-0.784615384615384,-0.769230769230768,
-0.753846153846153,-0.738461538461538,-0.723076923076922,-0.707692307692307,
-0.692307692307692,-0.676923076923076,-0.661538461538461,-0.646153846153846,
-0.63076923076923,-0.615384615384615,-0.6,-0.584615384615384,-0.569230769230769,
-0.553846153846154,-0.538461538461538,-0.523076923076923,-0.507692307692308,
-0.492307692307692,-0.476923076923077,-0.461538461538462,-0.446153846153846,
-0.430769230769231,-0.415384615384615,-0.4,-0.384615384615385,-0.369230769230769,
-0.353846153846154,-0.338461538461538,-0.323076923076923,-0.307692307692308,
-0.292307692307692,-0.276923076923077,-0.261538461538462,-0.246153846153846,
-0.230769230769231,-0.215384615384615,-0.2,-0.184615384615385,-0.169230769230769,
-0.153846153846154,-0.138461538461538,-0.123076923076923,-0.107692307692308,
-0.0923076923076923,-0.0769230769230769,-0.0615384615384615,-0.0461538461538462,
-0.0307692307692308,-0.0153846153846154,0.),(-1.,1.),.UNSPECIFIED.)
GEOMETRIC_REPRESENTATION_ITEM()
RATIONAL_B_SPLINE_SURFACE(((1.,1.),(1.,1.),(1.,1.),(1.,1.),(1.,1.),(1.,
1.),(1.,1.),(1.,1.),(1.,1.),(1.,1.),(1.,1.),(1.,1.),(1.,1.),(1.,1.),(1.,
1.),(1.,1.),(1.,1.),(1.,1.),(1.,1.),(1.,1.),(1.,1.),(1.,1.),(1.,1.),(1.,
1.),(1.,1.),(1.,1.),(1.,1.),(1.,1.),(1.,1.),(1.,1.),(1.,1.),(1.,1.),(1.,
1.),(1.,1.),(1.,1.),(1.,1.),(1.,1.),(1.,1.),(1.,1.),(1.,1.),(1.,1.),(1.,
1.),(1.,1.),(1.,1.),(1.,1.),(1.,1.),(1.,1.),(1.,1.),(1.,1.),(1.,1.),(1.,
1.),(1.,1.),(1.,1.),(1.,1.),(1.,1.),(1.,1.),(1.,1.),(1.,1.),(1.,1.),(1.,
1.),(1.,1.),(1.,1.),(1.,1.),(1.,1.),(1.,1.),(1.,1.),(1.,1.),(1.,1.),(1.,
1.),(1.,1.)))
REPRESENTATION_ITEM('')
SURFACE()
);
#48=(
BOUNDED_SURFACE()
B_SPLINE_SURFACE(5,1,((#33772,#33773),(#33774,#33775),(#33776,#33777),(#33778,
#33779),(#33780,#33781),(#33782,#33783),(#33784,#33785),(#33786,#33787),
(#33788,#33789),(#33790,#33791),(#33792,#33793),(#33794,#33795),(#33796,
#33797),(#33798,#33799),(#33800,#33801),(#33802,#33803),(#33804,#33805),
(#33806,#33807),(#33808,#33809),(#33810,#33811),(#33812,#33813),(#33814,
#33815),(#33816,#33817),(#33818,#33819),(#33820,#33821),(#33822,#33823),
(#33824,#33825),(#33826,#33827),(#33828,#33829),(#33830,#33831),(#33832,
#33833),(#33834,#33835),(#33836,#33837),(#33838,#33839),(#33840,#33841),
(#33842,#33843),(#33844,#33845),(#33846,#33847),(#33848,#33849),(#33850,
#33851),(#33852,#33853),(#33854,#33855),(#33856,#33857),(#33858,#33859),
(#33860,#33861),(#33862,#33863),(#33864,#33865),(#33866,#33867),(#33868,
#33869),(#33870,#33871),(#33872,#33873),(#33874,#33875),(#33876,#33877),
(#33878,#33879),(#33880,#33881),(#33882,#33883),(#33884,#33885),(#33886,
#33887),(#33888,#33889),(#33890,#33891),(#33892,#33893),(#33894,#33895),
(#33896,#33897),(#33898,#33899),(#33900,#33901),(#33902,#33903),(#33904,
#33905),(#33906,#33907),(#33908,#33909),(#33910,#33911)),.UNSPECIFIED.,
 .F.,.F.,.F.)
B_SPLINE_SURFACE_WITH_KNOTS((6,1,1,1,1,1,1,1,1,1,1,1,1,1,1,1,1,1,1,1,1,
1,1,1,1,1,1,1,1,1,1,1,1,1,1,1,1,1,1,1,1,1,1,1,1,1,1,1,1,1,1,1,1,1,1,1,1,
1,1,1,1,1,1,1,1,6),(2,2),(-1.,-0.984615384615383,-0.969230769230768,-0.953846153846152,
-0.938461538461537,-0.923076923076922,-0.907692307692306,-0.892307692307691,
-0.876923076923076,-0.86153846153846,-0.846153846153845,-0.83076923076923,
-0.815384615384614,-0.799999999999999,-0.784615384615384,-0.769230769230768,
-0.753846153846153,-0.738461538461538,-0.723076923076922,-0.707692307692307,
-0.692307692307692,-0.676923076923076,-0.661538461538461,-0.646153846153846,
-0.63076923076923,-0.615384615384615,-0.6,-0.584615384615384,-0.569230769230769,
-0.553846153846154,-0.538461538461538,-0.523076923076923,-0.507692307692308,
-0.492307692307692,-0.476923076923077,-0.461538461538462,-0.446153846153846,
-0.430769230769231,-0.415384615384615,-0.4,-0.384615384615385,-0.369230769230769,
-0.353846153846154,-0.338461538461538,-0.323076923076923,-0.307692307692308,
-0.292307692307692,-0.276923076923077,-0.261538461538462,-0.246153846153846,
-0.230769230769231,-0.215384615384615,-0.2,-0.184615384615385,-0.169230769230769,
-0.153846153846154,-0.138461538461538,-0.123076923076923,-0.107692307692308,
-0.0923076923076923,-0.0769230769230769,-0.0615384615384615,-0.0461538461538462,
-0.0307692307692308,-0.0153846153846154,0.),(-1.,1.),.UNSPECIFIED.)
GEOMETRIC_REPRESENTATION_ITEM()
RATIONAL_B_SPLINE_SURFACE(((1.,1.),(1.,1.),(1.,1.),(1.,1.),(1.,1.),(1.,
1.),(1.,1.),(1.,1.),(1.,1.),(1.,1.),(1.,1.),(1.,1.),(1.,1.),(1.,1.),(1.,
1.),(1.,1.),(1.,1.),(1.,1.),(1.,1.),(1.,1.),(1.,1.),(1.,1.),(1.,1.),(1.,
1.),(1.,1.),(1.,1.),(1.,1.),(1.,1.),(1.,1.),(1.,1.),(1.,1.),(1.,1.),(1.,
1.),(1.,1.),(1.,1.),(1.,1.),(1.,1.),(1.,1.),(1.,1.),(1.,1.),(1.,1.),(1.,
1.),(1.,1.),(1.,1.),(1.,1.),(1.,1.),(1.,1.),(1.,1.),(1.,1.),(1.,1.),(1.,
1.),(1.,1.),(1.,1.),(1.,1.),(1.,1.),(1.,1.),(1.,1.),(1.,1.),(1.,1.),(1.,
1.),(1.,1.),(1.,1.),(1.,1.),(1.,1.),(1.,1.),(1.,1.),(1.,1.),(1.,1.),(1.,
1.),(1.,1.)))
REPRESENTATION_ITEM('')
SURFACE()
);
#49=(
BOUNDED_SURFACE()
B_SPLINE_SURFACE(5,1,((#33988,#33989),(#33990,#33991),(#33992,#33993),(#33994,
#33995),(#33996,#33997),(#33998,#33999),(#34000,#34001),(#34002,#34003),
(#34004,#34005),(#34006,#34007),(#34008,#34009),(#34010,#34011),(#34012,
#34013),(#34014,#34015),(#34016,#34017),(#34018,#34019),(#34020,#34021),
(#34022,#34023),(#34024,#34025),(#34026,#34027),(#34028,#34029),(#34030,
#34031),(#34032,#34033),(#34034,#34035),(#34036,#34037),(#34038,#34039),
(#34040,#34041),(#34042,#34043),(#34044,#34045),(#34046,#34047),(#34048,
#34049),(#34050,#34051),(#34052,#34053),(#34054,#34055),(#34056,#34057),
(#34058,#34059),(#34060,#34061),(#34062,#34063),(#34064,#34065),(#34066,
#34067),(#34068,#34069),(#34070,#34071),(#34072,#34073),(#34074,#34075),
(#34076,#34077),(#34078,#34079),(#34080,#34081),(#34082,#34083),(#34084,
#34085),(#34086,#34087),(#34088,#34089),(#34090,#34091),(#34092,#34093),
(#34094,#34095),(#34096,#34097),(#34098,#34099),(#34100,#34101),(#34102,
#34103),(#34104,#34105),(#34106,#34107),(#34108,#34109),(#34110,#34111),
(#34112,#34113),(#34114,#34115),(#34116,#34117),(#34118,#34119),(#34120,
#34121),(#34122,#34123),(#34124,#34125),(#34126,#34127)),.UNSPECIFIED.,
 .F.,.F.,.F.)
B_SPLINE_SURFACE_WITH_KNOTS((6,1,1,1,1,1,1,1,1,1,1,1,1,1,1,1,1,1,1,1,1,
1,1,1,1,1,1,1,1,1,1,1,1,1,1,1,1,1,1,1,1,1,1,1,1,1,1,1,1,1,1,1,1,1,1,1,1,
1,1,1,1,1,1,1,1,6),(2,2),(-1.,-0.984615384615383,-0.969230769230768,-0.953846153846152,
-0.938461538461537,-0.923076923076922,-0.907692307692306,-0.892307692307691,
-0.876923076923076,-0.86153846153846,-0.846153846153845,-0.83076923076923,
-0.815384615384614,-0.799999999999999,-0.784615384615384,-0.769230769230768,
-0.753846153846153,-0.738461538461538,-0.723076923076922,-0.707692307692307,
-0.692307692307692,-0.676923076923076,-0.661538461538461,-0.646153846153846,
-0.63076923076923,-0.615384615384615,-0.6,-0.584615384615384,-0.569230769230769,
-0.553846153846154,-0.538461538461538,-0.523076923076923,-0.507692307692308,
-0.492307692307692,-0.476923076923077,-0.461538461538462,-0.446153846153846,
-0.430769230769231,-0.415384615384615,-0.4,-0.384615384615385,-0.369230769230769,
-0.353846153846154,-0.338461538461538,-0.323076923076923,-0.307692307692308,
-0.292307692307692,-0.276923076923077,-0.261538461538462,-0.246153846153846,
-0.230769230769231,-0.215384615384615,-0.2,-0.184615384615385,-0.169230769230769,
-0.153846153846154,-0.138461538461538,-0.123076923076923,-0.107692307692308,
-0.0923076923076923,-0.0769230769230769,-0.0615384615384615,-0.0461538461538462,
-0.0307692307692308,-0.0153846153846154,0.),(-1.,1.),.UNSPECIFIED.)
GEOMETRIC_REPRESENTATION_ITEM()
RATIONAL_B_SPLINE_SURFACE(((1.,1.),(1.,1.),(1.,1.),(1.,1.),(1.,1.),(1.,
1.),(1.,1.),(1.,1.),(1.,1.),(1.,1.),(1.,1.),(1.,1.),(1.,1.),(1.,1.),(1.,
1.),(1.,1.),(1.,1.),(1.,1.),(1.,1.),(1.,1.),(1.,1.),(1.,1.),(1.,1.),(1.,
1.),(1.,1.),(1.,1.),(1.,1.),(1.,1.),(1.,1.),(1.,1.),(1.,1.),(1.,1.),(1.,
1.),(1.,1.),(1.,1.),(1.,1.),(1.,1.),(1.,1.),(1.,1.),(1.,1.),(1.,1.),(1.,
1.),(1.,1.),(1.,1.),(1.,1.),(1.,1.),(1.,1.),(1.,1.),(1.,1.),(1.,1.),(1.,
1.),(1.,1.),(1.,1.),(1.,1.),(1.,1.),(1.,1.),(1.,1.),(1.,1.),(1.,1.),(1.,
1.),(1.,1.),(1.,1.),(1.,1.),(1.,1.),(1.,1.),(1.,1.),(1.,1.),(1.,1.),(1.,
1.),(1.,1.)))
REPRESENTATION_ITEM('')
SURFACE()
);
#50=(
BOUNDED_SURFACE()
B_SPLINE_SURFACE(5,1,((#34204,#34205),(#34206,#34207),(#34208,#34209),(#34210,
#34211),(#34212,#34213),(#34214,#34215),(#34216,#34217),(#34218,#34219),
(#34220,#34221),(#34222,#34223),(#34224,#34225),(#34226,#34227),(#34228,
#34229),(#34230,#34231),(#34232,#34233),(#34234,#34235),(#34236,#34237),
(#34238,#34239),(#34240,#34241),(#34242,#34243),(#34244,#34245),(#34246,
#34247),(#34248,#34249),(#34250,#34251),(#34252,#34253),(#34254,#34255),
(#34256,#34257),(#34258,#34259),(#34260,#34261),(#34262,#34263),(#34264,
#34265),(#34266,#34267),(#34268,#34269),(#34270,#34271),(#34272,#34273),
(#34274,#34275),(#34276,#34277),(#34278,#34279),(#34280,#34281),(#34282,
#34283),(#34284,#34285),(#34286,#34287),(#34288,#34289),(#34290,#34291),
(#34292,#34293),(#34294,#34295),(#34296,#34297),(#34298,#34299),(#34300,
#34301),(#34302,#34303),(#34304,#34305),(#34306,#34307),(#34308,#34309),
(#34310,#34311),(#34312,#34313),(#34314,#34315),(#34316,#34317),(#34318,
#34319),(#34320,#34321),(#34322,#34323),(#34324,#34325),(#34326,#34327),
(#34328,#34329),(#34330,#34331),(#34332,#34333),(#34334,#34335),(#34336,
#34337),(#34338,#34339),(#34340,#34341),(#34342,#34343)),.UNSPECIFIED.,
 .F.,.F.,.F.)
B_SPLINE_SURFACE_WITH_KNOTS((6,1,1,1,1,1,1,1,1,1,1,1,1,1,1,1,1,1,1,1,1,
1,1,1,1,1,1,1,1,1,1,1,1,1,1,1,1,1,1,1,1,1,1,1,1,1,1,1,1,1,1,1,1,1,1,1,1,
1,1,1,1,1,1,1,1,6),(2,2),(-1.,-0.984615384615383,-0.969230769230768,-0.953846153846152,
-0.938461538461537,-0.923076923076922,-0.907692307692306,-0.892307692307691,
-0.876923076923076,-0.86153846153846,-0.846153846153845,-0.83076923076923,
-0.815384615384614,-0.799999999999999,-0.784615384615384,-0.769230769230768,
-0.753846153846153,-0.738461538461538,-0.723076923076922,-0.707692307692307,
-0.692307692307692,-0.676923076923076,-0.661538461538461,-0.646153846153846,
-0.63076923076923,-0.615384615384615,-0.6,-0.584615384615384,-0.569230769230769,
-0.553846153846154,-0.538461538461538,-0.523076923076923,-0.507692307692308,
-0.492307692307692,-0.476923076923077,-0.461538461538462,-0.446153846153846,
-0.430769230769231,-0.415384615384615,-0.4,-0.384615384615385,-0.369230769230769,
-0.353846153846154,-0.338461538461538,-0.323076923076923,-0.307692307692308,
-0.292307692307692,-0.276923076923077,-0.261538461538462,-0.246153846153846,
-0.230769230769231,-0.215384615384615,-0.2,-0.184615384615385,-0.169230769230769,
-0.153846153846154,-0.138461538461538,-0.123076923076923,-0.107692307692308,
-0.0923076923076923,-0.0769230769230769,-0.0615384615384615,-0.0461538461538462,
-0.0307692307692308,-0.0153846153846154,0.),(-1.,1.),.UNSPECIFIED.)
GEOMETRIC_REPRESENTATION_ITEM()
RATIONAL_B_SPLINE_SURFACE(((1.,1.),(1.,1.),(1.,1.),(1.,1.),(1.,1.),(1.,
1.),(1.,1.),(1.,1.),(1.,1.),(1.,1.),(1.,1.),(1.,1.),(1.,1.),(1.,1.),(1.,
1.),(1.,1.),(1.,1.),(1.,1.),(1.,1.),(1.,1.),(1.,1.),(1.,1.),(1.,1.),(1.,
1.),(1.,1.),(1.,1.),(1.,1.),(1.,1.),(1.,1.),(1.,1.),(1.,1.),(1.,1.),(1.,
1.),(1.,1.),(1.,1.),(1.,1.),(1.,1.),(1.,1.),(1.,1.),(1.,1.),(1.,1.),(1.,
1.),(1.,1.),(1.,1.),(1.,1.),(1.,1.),(1.,1.),(1.,1.),(1.,1.),(1.,1.),(1.,
1.),(1.,1.),(1.,1.),(1.,1.),(1.,1.),(1.,1.),(1.,1.),(1.,1.),(1.,1.),(1.,
1.),(1.,1.),(1.,1.),(1.,1.),(1.,1.),(1.,1.),(1.,1.),(1.,1.),(1.,1.),(1.,
1.),(1.,1.)))
REPRESENTATION_ITEM('')
SURFACE()
);
#51=(
BOUNDED_CURVE()
B_SPLINE_CURVE(5,(#22852,#22853,#22854,#22855,#22856,#22857,#22858,#22859,
#22860,#22861,#22862,#22863,#22864,#22865,#22866,#22867,#22868,#22869,#22870,
#22871,#22872,#22873,#22874,#22875,#22876,#22877,#22878,#22879,#22880,#22881,
#22882,#22883,#22884,#22885,#22886,#22887,#22888,#22889,#22890,#22891,#22892,
#22893,#22894,#22895,#22896,#22897,#22898,#22899,#22900,#22901,#22902,#22903,
#22904,#22905,#22906,#22907,#22908,#22909,#22910,#22911,#22912,#22913,#22914,
#22915,#22916,#22917,#22918,#22919,#22920,#22921),.UNSPECIFIED.,.F.,.F.)
B_SPLINE_CURVE_WITH_KNOTS((6,1,1,1,1,1,1,1,1,1,1,1,1,1,1,1,1,1,1,1,1,1,
1,1,1,1,1,1,1,1,1,1,1,1,1,1,1,1,1,1,1,1,1,1,1,1,1,1,1,1,1,1,1,1,1,1,1,1,
1,1,1,1,1,1,1,6),(0.,0.0153846153846154,0.0307692307692308,0.0461538461538462,
0.0615384615384615,0.0769230769230769,0.0923076923076923,0.107692307692308,
0.123076923076923,0.138461538461538,0.153846153846154,0.169230769230769,
0.184615384615385,0.2,0.215384615384615,0.230769230769231,0.246153846153846,
0.261538461538462,0.276923076923077,0.292307692307692,0.307692307692308,
0.323076923076923,0.338461538461538,0.353846153846154,0.369230769230769,
0.384615384615385,0.4,0.415384615384615,0.430769230769231,0.446153846153846,
0.461538461538462,0.476923076923077,0.492307692307692,0.507692307692308,
0.523076923076923,0.538461538461538,0.553846153846154,0.569230769230769,
0.584615384615384,0.6,0.615384615384615,0.63076923076923,0.646153846153846,
0.661538461538461,0.676923076923076,0.692307692307692,0.707692307692307,
0.723076923076922,0.738461538461538,0.753846153846153,0.769230769230768,
0.784615384615384,0.799999999999999,0.815384615384614,0.83076923076923,
0.846153846153845,0.86153846153846,0.876923076923076,0.892307692307691,
0.907692307692306,0.923076923076922,0.938461538461537,0.953846153846152,
0.969230769230768,0.984615384615383,1.),.UNSPECIFIED.)
CURVE()
GEOMETRIC_REPRESENTATION_ITEM()
RATIONAL_B_SPLINE_CURVE((1.,1.,1.,1.,1.,1.,1.,1.,1.,1.,1.,1.,1.,1.,1.,1.,
1.,1.,1.,1.,1.,1.,1.,1.,1.,1.,1.,1.,1.,1.,1.,1.,1.,1.,1.,1.,1.,1.,1.,1.,
1.,1.,1.,1.,1.,1.,1.,1.,1.,1.,1.,1.,1.,1.,1.,1.,1.,1.,1.,1.,1.,1.,1.,1.,
1.,1.,1.,1.,1.,1.))
REPRESENTATION_ITEM('')
);
#52=(
BOUNDED_CURVE()
B_SPLINE_CURVE(5,(#22925,#22926,#22927,#22928,#22929,#22930,#22931,#22932,
#22933,#22934,#22935,#22936,#22937,#22938,#22939,#22940,#22941,#22942,#22943,
#22944,#22945,#22946,#22947,#22948,#22949,#22950,#22951,#22952,#22953,#22954,
#22955,#22956,#22957,#22958,#22959,#22960,#22961,#22962,#22963,#22964,#22965,
#22966,#22967,#22968,#22969,#22970,#22971,#22972,#22973,#22974,#22975,#22976,
#22977,#22978,#22979,#22980,#22981,#22982,#22983,#22984,#22985,#22986,#22987,
#22988,#22989,#22990,#22991,#22992,#22993,#22994),.UNSPECIFIED.,.F.,.F.)
B_SPLINE_CURVE_WITH_KNOTS((6,1,1,1,1,1,1,1,1,1,1,1,1,1,1,1,1,1,1,1,1,1,
1,1,1,1,1,1,1,1,1,1,1,1,1,1,1,1,1,1,1,1,1,1,1,1,1,1,1,1,1,1,1,1,1,1,1,1,
1,1,1,1,1,1,1,6),(0.,0.0153846153846154,0.0307692307692308,0.0461538461538462,
0.0615384615384615,0.0769230769230769,0.0923076923076923,0.107692307692308,
0.123076923076923,0.138461538461538,0.153846153846154,0.169230769230769,
0.184615384615385,0.2,0.215384615384615,0.230769230769231,0.246153846153846,
0.261538461538462,0.276923076923077,0.292307692307692,0.307692307692308,
0.323076923076923,0.338461538461538,0.353846153846154,0.369230769230769,
0.384615384615385,0.4,0.415384615384615,0.430769230769231,0.446153846153846,
0.461538461538462,0.476923076923077,0.492307692307692,0.507692307692308,
0.523076923076923,0.538461538461538,0.553846153846154,0.569230769230769,
0.584615384615384,0.6,0.615384615384615,0.63076923076923,0.646153846153846,
0.661538461538461,0.676923076923076,0.692307692307692,0.707692307692307,
0.723076923076922,0.738461538461538,0.753846153846153,0.769230769230768,
0.784615384615384,0.799999999999999,0.815384615384614,0.83076923076923,
0.846153846153845,0.86153846153846,0.876923076923076,0.892307692307691,
0.907692307692306,0.923076923076922,0.938461538461537,0.953846153846152,
0.969230769230768,0.984615384615383,1.),.UNSPECIFIED.)
CURVE()
GEOMETRIC_REPRESENTATION_ITEM()
RATIONAL_B_SPLINE_CURVE((1.,1.,1.,1.,1.,1.,1.,1.,1.,1.,1.,1.,1.,1.,1.,1.,
1.,1.,1.,1.,1.,1.,1.,1.,1.,1.,1.,1.,1.,1.,1.,1.,1.,1.,1.,1.,1.,1.,1.,1.,
1.,1.,1.,1.,1.,1.,1.,1.,1.,1.,1.,1.,1.,1.,1.,1.,1.,1.,1.,1.,1.,1.,1.,1.,
1.,1.,1.,1.,1.,1.))
REPRESENTATION_ITEM('')
);
#53=(
BOUNDED_CURVE()
B_SPLINE_CURVE(5,(#22998,#22999,#23000,#23001,#23002,#23003,#23004,#23005,
#23006,#23007,#23008,#23009,#23010,#23011,#23012,#23013,#23014,#23015,#23016,
#23017,#23018,#23019,#23020,#23021,#23022,#23023,#23024,#23025,#23026,#23027,
#23028,#23029,#23030,#23031,#23032,#23033,#23034,#23035,#23036,#23037,#23038,
#23039,#23040,#23041,#23042,#23043,#23044,#23045,#23046,#23047,#23048,#23049,
#23050,#23051,#23052,#23053,#23054,#23055,#23056,#23057,#23058,#23059,#23060,
#23061,#23062,#23063,#23064,#23065,#23066,#23067),.UNSPECIFIED.,.F.,.F.)
B_SPLINE_CURVE_WITH_KNOTS((6,1,1,1,1,1,1,1,1,1,1,1,1,1,1,1,1,1,1,1,1,1,
1,1,1,1,1,1,1,1,1,1,1,1,1,1,1,1,1,1,1,1,1,1,1,1,1,1,1,1,1,1,1,1,1,1,1,1,
1,1,1,1,1,1,1,6),(0.,0.0153846153846154,0.0307692307692308,0.0461538461538462,
0.0615384615384615,0.0769230769230769,0.0923076923076923,0.107692307692308,
0.123076923076923,0.138461538461538,0.153846153846154,0.169230769230769,
0.184615384615385,0.2,0.215384615384615,0.230769230769231,0.246153846153846,
0.261538461538462,0.276923076923077,0.292307692307692,0.307692307692308,
0.323076923076923,0.338461538461538,0.353846153846154,0.369230769230769,
0.384615384615385,0.4,0.415384615384615,0.430769230769231,0.446153846153846,
0.461538461538462,0.476923076923077,0.492307692307692,0.507692307692308,
0.523076923076923,0.538461538461538,0.553846153846154,0.569230769230769,
0.584615384615384,0.6,0.615384615384615,0.63076923076923,0.646153846153846,
0.661538461538461,0.676923076923076,0.692307692307692,0.707692307692307,
0.723076923076922,0.738461538461538,0.753846153846153,0.769230769230768,
0.784615384615384,0.799999999999999,0.815384615384614,0.83076923076923,
0.846153846153845,0.86153846153846,0.876923076923076,0.892307692307691,
0.907692307692306,0.923076923076922,0.938461538461537,0.953846153846152,
0.969230769230768,0.984615384615383,1.),.UNSPECIFIED.)
CURVE()
GEOMETRIC_REPRESENTATION_ITEM()
RATIONAL_B_SPLINE_CURVE((1.,1.,1.,1.,1.,1.,1.,1.,1.,1.,1.,1.,1.,1.,1.,1.,
1.,1.,1.,1.,1.,1.,1.,1.,1.,1.,1.,1.,1.,1.,1.,1.,1.,1.,1.,1.,1.,1.,1.,1.,
1.,1.,1.,1.,1.,1.,1.,1.,1.,1.,1.,1.,1.,1.,1.,1.,1.,1.,1.,1.,1.,1.,1.,1.,
1.,1.,1.,1.,1.,1.))
REPRESENTATION_ITEM('')
);
#54=(
BOUNDED_CURVE()
B_SPLINE_CURVE(5,(#23071,#23072,#23073,#23074,#23075,#23076,#23077,#23078,
#23079,#23080,#23081,#23082,#23083,#23084,#23085,#23086,#23087,#23088,#23089,
#23090,#23091,#23092,#23093,#23094,#23095,#23096,#23097,#23098,#23099,#23100,
#23101,#23102,#23103,#23104,#23105,#23106,#23107,#23108,#23109,#23110,#23111,
#23112,#23113,#23114,#23115,#23116,#23117,#23118,#23119,#23120,#23121,#23122,
#23123,#23124,#23125,#23126,#23127,#23128,#23129,#23130,#23131,#23132,#23133,
#23134,#23135,#23136,#23137,#23138,#23139,#23140),.UNSPECIFIED.,.F.,.F.)
B_SPLINE_CURVE_WITH_KNOTS((6,1,1,1,1,1,1,1,1,1,1,1,1,1,1,1,1,1,1,1,1,1,
1,1,1,1,1,1,1,1,1,1,1,1,1,1,1,1,1,1,1,1,1,1,1,1,1,1,1,1,1,1,1,1,1,1,1,1,
1,1,1,1,1,1,1,6),(0.,0.0153846153846154,0.0307692307692308,0.0461538461538462,
0.0615384615384615,0.0769230769230769,0.0923076923076923,0.107692307692308,
0.123076923076923,0.138461538461538,0.153846153846154,0.169230769230769,
0.184615384615385,0.2,0.215384615384615,0.230769230769231,0.246153846153846,
0.261538461538462,0.276923076923077,0.292307692307692,0.307692307692308,
0.323076923076923,0.338461538461538,0.353846153846154,0.369230769230769,
0.384615384615385,0.4,0.415384615384615,0.430769230769231,0.446153846153846,
0.461538461538462,0.476923076923077,0.492307692307692,0.507692307692308,
0.523076923076923,0.538461538461538,0.553846153846154,0.569230769230769,
0.584615384615384,0.6,0.615384615384615,0.63076923076923,0.646153846153846,
0.661538461538461,0.676923076923076,0.692307692307692,0.707692307692307,
0.723076923076922,0.738461538461538,0.753846153846153,0.769230769230768,
0.784615384615384,0.799999999999999,0.815384615384614,0.83076923076923,
0.846153846153845,0.86153846153846,0.876923076923076,0.892307692307691,
0.907692307692306,0.923076923076922,0.938461538461537,0.953846153846152,
0.969230769230768,0.984615384615383,1.),.UNSPECIFIED.)
CURVE()
GEOMETRIC_REPRESENTATION_ITEM()
RATIONAL_B_SPLINE_CURVE((1.,1.,1.,1.,1.,1.,1.,1.,1.,1.,1.,1.,1.,1.,1.,1.,
1.,1.,1.,1.,1.,1.,1.,1.,1.,1.,1.,1.,1.,1.,1.,1.,1.,1.,1.,1.,1.,1.,1.,1.,
1.,1.,1.,1.,1.,1.,1.,1.,1.,1.,1.,1.,1.,1.,1.,1.,1.,1.,1.,1.,1.,1.,1.,1.,
1.,1.,1.,1.,1.,1.))
REPRESENTATION_ITEM('')
);
#55=(
BOUNDED_CURVE()
B_SPLINE_CURVE(5,(#23144,#23145,#23146,#23147,#23148,#23149,#23150,#23151,
#23152,#23153,#23154,#23155,#23156,#23157,#23158,#23159,#23160,#23161,#23162,
#23163,#23164,#23165,#23166,#23167,#23168,#23169,#23170,#23171,#23172,#23173,
#23174,#23175,#23176,#23177,#23178,#23179,#23180,#23181,#23182,#23183,#23184,
#23185,#23186,#23187,#23188,#23189,#23190,#23191,#23192,#23193,#23194,#23195,
#23196,#23197,#23198,#23199,#23200,#23201,#23202,#23203,#23204,#23205,#23206,
#23207,#23208,#23209,#23210,#23211,#23212,#23213),.UNSPECIFIED.,.F.,.F.)
B_SPLINE_CURVE_WITH_KNOTS((6,1,1,1,1,1,1,1,1,1,1,1,1,1,1,1,1,1,1,1,1,1,
1,1,1,1,1,1,1,1,1,1,1,1,1,1,1,1,1,1,1,1,1,1,1,1,1,1,1,1,1,1,1,1,1,1,1,1,
1,1,1,1,1,1,1,6),(0.,0.0153846153846154,0.0307692307692308,0.0461538461538462,
0.0615384615384615,0.0769230769230769,0.0923076923076923,0.107692307692308,
0.123076923076923,0.138461538461538,0.153846153846154,0.169230769230769,
0.184615384615385,0.2,0.215384615384615,0.230769230769231,0.246153846153846,
0.261538461538462,0.276923076923077,0.292307692307692,0.307692307692308,
0.323076923076923,0.338461538461538,0.353846153846154,0.369230769230769,
0.384615384615385,0.4,0.415384615384615,0.430769230769231,0.446153846153846,
0.461538461538462,0.476923076923077,0.492307692307692,0.507692307692308,
0.523076923076923,0.538461538461538,0.553846153846154,0.569230769230769,
0.584615384615384,0.6,0.615384615384615,0.63076923076923,0.646153846153846,
0.661538461538461,0.676923076923076,0.692307692307692,0.707692307692307,
0.723076923076922,0.738461538461538,0.753846153846153,0.769230769230768,
0.784615384615384,0.799999999999999,0.815384615384614,0.83076923076923,
0.846153846153845,0.86153846153846,0.876923076923076,0.892307692307691,
0.907692307692306,0.923076923076922,0.938461538461537,0.953846153846152,
0.969230769230768,0.984615384615383,1.),.UNSPECIFIED.)
CURVE()
GEOMETRIC_REPRESENTATION_ITEM()
RATIONAL_B_SPLINE_CURVE((1.,1.,1.,1.,1.,1.,1.,1.,1.,1.,1.,1.,1.,1.,1.,1.,
1.,1.,1.,1.,1.,1.,1.,1.,1.,1.,1.,1.,1.,1.,1.,1.,1.,1.,1.,1.,1.,1.,1.,1.,
1.,1.,1.,1.,1.,1.,1.,1.,1.,1.,1.,1.,1.,1.,1.,1.,1.,1.,1.,1.,1.,1.,1.,1.,
1.,1.,1.,1.,1.,1.))
REPRESENTATION_ITEM('')
);
#56=(
BOUNDED_CURVE()
B_SPLINE_CURVE(5,(#23217,#23218,#23219,#23220,#23221,#23222,#23223,#23224,
#23225,#23226,#23227,#23228,#23229,#23230,#23231,#23232,#23233,#23234,#23235,
#23236,#23237,#23238,#23239,#23240,#23241,#23242,#23243,#23244,#23245,#23246,
#23247,#23248,#23249,#23250,#23251,#23252,#23253,#23254,#23255,#23256,#23257,
#23258,#23259,#23260,#23261,#23262,#23263,#23264,#23265,#23266,#23267,#23268,
#23269,#23270,#23271,#23272,#23273,#23274,#23275,#23276,#23277,#23278,#23279,
#23280,#23281,#23282,#23283,#23284,#23285,#23286),.UNSPECIFIED.,.F.,.F.)
B_SPLINE_CURVE_WITH_KNOTS((6,1,1,1,1,1,1,1,1,1,1,1,1,1,1,1,1,1,1,1,1,1,
1,1,1,1,1,1,1,1,1,1,1,1,1,1,1,1,1,1,1,1,1,1,1,1,1,1,1,1,1,1,1,1,1,1,1,1,
1,1,1,1,1,1,1,6),(0.,0.0153846153846154,0.0307692307692308,0.0461538461538462,
0.0615384615384615,0.0769230769230769,0.0923076923076923,0.107692307692308,
0.123076923076923,0.138461538461538,0.153846153846154,0.169230769230769,
0.184615384615385,0.2,0.215384615384615,0.230769230769231,0.246153846153846,
0.261538461538462,0.276923076923077,0.292307692307692,0.307692307692308,
0.323076923076923,0.338461538461538,0.353846153846154,0.369230769230769,
0.384615384615385,0.4,0.415384615384615,0.430769230769231,0.446153846153846,
0.461538461538462,0.476923076923077,0.492307692307692,0.507692307692308,
0.523076923076923,0.538461538461538,0.553846153846154,0.569230769230769,
0.584615384615384,0.6,0.615384615384615,0.63076923076923,0.646153846153846,
0.661538461538461,0.676923076923076,0.692307692307692,0.707692307692307,
0.723076923076922,0.738461538461538,0.753846153846153,0.769230769230768,
0.784615384615384,0.799999999999999,0.815384615384614,0.83076923076923,
0.846153846153845,0.86153846153846,0.876923076923076,0.892307692307691,
0.907692307692306,0.923076923076922,0.938461538461537,0.953846153846152,
0.969230769230768,0.984615384615383,1.),.UNSPECIFIED.)
CURVE()
GEOMETRIC_REPRESENTATION_ITEM()
RATIONAL_B_SPLINE_CURVE((1.,1.,1.,1.,1.,1.,1.,1.,1.,1.,1.,1.,1.,1.,1.,1.,
1.,1.,1.,1.,1.,1.,1.,1.,1.,1.,1.,1.,1.,1.,1.,1.,1.,1.,1.,1.,1.,1.,1.,1.,
1.,1.,1.,1.,1.,1.,1.,1.,1.,1.,1.,1.,1.,1.,1.,1.,1.,1.,1.,1.,1.,1.,1.,1.,
1.,1.,1.,1.,1.,1.))
REPRESENTATION_ITEM('')
);
#57=(
BOUNDED_CURVE()
B_SPLINE_CURVE(5,(#23290,#23291,#23292,#23293,#23294,#23295,#23296,#23297,
#23298,#23299,#23300,#23301,#23302,#23303,#23304,#23305,#23306,#23307,#23308,
#23309,#23310,#23311,#23312,#23313,#23314,#23315,#23316,#23317,#23318,#23319,
#23320,#23321,#23322,#23323,#23324,#23325,#23326,#23327,#23328,#23329,#23330,
#23331,#23332,#23333,#23334,#23335,#23336,#23337,#23338,#23339,#23340,#23341,
#23342,#23343,#23344,#23345,#23346,#23347,#23348,#23349,#23350,#23351,#23352,
#23353,#23354,#23355,#23356,#23357,#23358,#23359),.UNSPECIFIED.,.F.,.F.)
B_SPLINE_CURVE_WITH_KNOTS((6,1,1,1,1,1,1,1,1,1,1,1,1,1,1,1,1,1,1,1,1,1,
1,1,1,1,1,1,1,1,1,1,1,1,1,1,1,1,1,1,1,1,1,1,1,1,1,1,1,1,1,1,1,1,1,1,1,1,
1,1,1,1,1,1,1,6),(0.,0.0153846153846154,0.0307692307692308,0.0461538461538462,
0.0615384615384615,0.0769230769230769,0.0923076923076923,0.107692307692308,
0.123076923076923,0.138461538461538,0.153846153846154,0.169230769230769,
0.184615384615385,0.2,0.215384615384615,0.230769230769231,0.246153846153846,
0.261538461538462,0.276923076923077,0.292307692307692,0.307692307692308,
0.323076923076923,0.338461538461538,0.353846153846154,0.369230769230769,
0.384615384615385,0.4,0.415384615384615,0.430769230769231,0.446153846153846,
0.461538461538462,0.476923076923077,0.492307692307692,0.507692307692308,
0.523076923076923,0.538461538461538,0.553846153846154,0.569230769230769,
0.584615384615384,0.6,0.615384615384615,0.63076923076923,0.646153846153846,
0.661538461538461,0.676923076923076,0.692307692307692,0.707692307692307,
0.723076923076922,0.738461538461538,0.753846153846153,0.769230769230768,
0.784615384615384,0.799999999999999,0.815384615384614,0.83076923076923,
0.846153846153845,0.86153846153846,0.876923076923076,0.892307692307691,
0.907692307692306,0.923076923076922,0.938461538461537,0.953846153846152,
0.969230769230768,0.984615384615383,1.),.UNSPECIFIED.)
CURVE()
GEOMETRIC_REPRESENTATION_ITEM()
RATIONAL_B_SPLINE_CURVE((1.,1.,1.,1.,1.,1.,1.,1.,1.,1.,1.,1.,1.,1.,1.,1.,
1.,1.,1.,1.,1.,1.,1.,1.,1.,1.,1.,1.,1.,1.,1.,1.,1.,1.,1.,1.,1.,1.,1.,1.,
1.,1.,1.,1.,1.,1.,1.,1.,1.,1.,1.,1.,1.,1.,1.,1.,1.,1.,1.,1.,1.,1.,1.,1.,
1.,1.,1.,1.,1.,1.))
REPRESENTATION_ITEM('')
);
#58=(
BOUNDED_CURVE()
B_SPLINE_CURVE(5,(#23363,#23364,#23365,#23366,#23367,#23368,#23369,#23370,
#23371,#23372,#23373,#23374,#23375,#23376,#23377,#23378,#23379,#23380,#23381,
#23382,#23383,#23384,#23385,#23386,#23387,#23388,#23389,#23390,#23391,#23392,
#23393,#23394,#23395,#23396,#23397,#23398,#23399,#23400,#23401,#23402,#23403,
#23404,#23405,#23406,#23407,#23408,#23409,#23410,#23411,#23412,#23413,#23414,
#23415,#23416,#23417,#23418,#23419,#23420,#23421,#23422,#23423,#23424,#23425,
#23426,#23427,#23428,#23429,#23430,#23431,#23432),.UNSPECIFIED.,.F.,.F.)
B_SPLINE_CURVE_WITH_KNOTS((6,1,1,1,1,1,1,1,1,1,1,1,1,1,1,1,1,1,1,1,1,1,
1,1,1,1,1,1,1,1,1,1,1,1,1,1,1,1,1,1,1,1,1,1,1,1,1,1,1,1,1,1,1,1,1,1,1,1,
1,1,1,1,1,1,1,6),(0.,0.0153846153846154,0.0307692307692308,0.0461538461538462,
0.0615384615384615,0.0769230769230769,0.0923076923076923,0.107692307692308,
0.123076923076923,0.138461538461538,0.153846153846154,0.169230769230769,
0.184615384615385,0.2,0.215384615384615,0.230769230769231,0.246153846153846,
0.261538461538462,0.276923076923077,0.292307692307692,0.307692307692308,
0.323076923076923,0.338461538461538,0.353846153846154,0.369230769230769,
0.384615384615385,0.4,0.415384615384615,0.430769230769231,0.446153846153846,
0.461538461538462,0.476923076923077,0.492307692307692,0.507692307692308,
0.523076923076923,0.538461538461538,0.553846153846154,0.569230769230769,
0.584615384615384,0.6,0.615384615384615,0.63076923076923,0.646153846153846,
0.661538461538461,0.676923076923076,0.692307692307692,0.707692307692307,
0.723076923076922,0.738461538461538,0.753846153846153,0.769230769230768,
0.784615384615384,0.799999999999999,0.815384615384614,0.83076923076923,
0.846153846153845,0.86153846153846,0.876923076923076,0.892307692307691,
0.907692307692306,0.923076923076922,0.938461538461537,0.953846153846152,
0.969230769230768,0.984615384615383,1.),.UNSPECIFIED.)
CURVE()
GEOMETRIC_REPRESENTATION_ITEM()
RATIONAL_B_SPLINE_CURVE((1.,1.,1.,1.,1.,1.,1.,1.,1.,1.,1.,1.,1.,1.,1.,1.,
1.,1.,1.,1.,1.,1.,1.,1.,1.,1.,1.,1.,1.,1.,1.,1.,1.,1.,1.,1.,1.,1.,1.,1.,
1.,1.,1.,1.,1.,1.,1.,1.,1.,1.,1.,1.,1.,1.,1.,1.,1.,1.,1.,1.,1.,1.,1.,1.,
1.,1.,1.,1.,1.,1.))
REPRESENTATION_ITEM('')
);
#59=(
BOUNDED_CURVE()
B_SPLINE_CURVE(5,(#23436,#23437,#23438,#23439,#23440,#23441,#23442,#23443,
#23444,#23445,#23446,#23447,#23448,#23449,#23450,#23451,#23452,#23453,#23454,
#23455,#23456,#23457,#23458,#23459,#23460,#23461,#23462,#23463,#23464,#23465,
#23466,#23467,#23468,#23469,#23470,#23471,#23472,#23473,#23474,#23475,#23476,
#23477,#23478,#23479,#23480,#23481,#23482,#23483,#23484,#23485,#23486,#23487,
#23488,#23489,#23490,#23491,#23492,#23493,#23494,#23495,#23496,#23497,#23498,
#23499,#23500,#23501,#23502,#23503,#23504,#23505),.UNSPECIFIED.,.F.,.F.)
B_SPLINE_CURVE_WITH_KNOTS((6,1,1,1,1,1,1,1,1,1,1,1,1,1,1,1,1,1,1,1,1,1,
1,1,1,1,1,1,1,1,1,1,1,1,1,1,1,1,1,1,1,1,1,1,1,1,1,1,1,1,1,1,1,1,1,1,1,1,
1,1,1,1,1,1,1,6),(0.,0.0153846153846154,0.0307692307692308,0.0461538461538462,
0.0615384615384615,0.0769230769230769,0.0923076923076923,0.107692307692308,
0.123076923076923,0.138461538461538,0.153846153846154,0.169230769230769,
0.184615384615385,0.2,0.215384615384615,0.230769230769231,0.246153846153846,
0.261538461538462,0.276923076923077,0.292307692307692,0.307692307692308,
0.323076923076923,0.338461538461538,0.353846153846154,0.369230769230769,
0.384615384615385,0.4,0.415384615384615,0.430769230769231,0.446153846153846,
0.461538461538462,0.476923076923077,0.492307692307692,0.507692307692308,
0.523076923076923,0.538461538461538,0.553846153846154,0.569230769230769,
0.584615384615384,0.6,0.615384615384615,0.63076923076923,0.646153846153846,
0.661538461538461,0.676923076923076,0.692307692307692,0.707692307692307,
0.723076923076922,0.738461538461538,0.753846153846153,0.769230769230768,
0.784615384615384,0.799999999999999,0.815384615384614,0.83076923076923,
0.846153846153845,0.86153846153846,0.876923076923076,0.892307692307691,
0.907692307692306,0.923076923076922,0.938461538461537,0.953846153846152,
0.969230769230768,0.984615384615383,1.),.UNSPECIFIED.)
CURVE()
GEOMETRIC_REPRESENTATION_ITEM()
RATIONAL_B_SPLINE_CURVE((1.,1.,1.,1.,1.,1.,1.,1.,1.,1.,1.,1.,1.,1.,1.,1.,
1.,1.,1.,1.,1.,1.,1.,1.,1.,1.,1.,1.,1.,1.,1.,1.,1.,1.,1.,1.,1.,1.,1.,1.,
1.,1.,1.,1.,1.,1.,1.,1.,1.,1.,1.,1.,1.,1.,1.,1.,1.,1.,1.,1.,1.,1.,1.,1.,
1.,1.,1.,1.,1.,1.))
REPRESENTATION_ITEM('')
);
#60=(
BOUNDED_CURVE()
B_SPLINE_CURVE(5,(#23509,#23510,#23511,#23512,#23513,#23514,#23515,#23516,
#23517,#23518,#23519,#23520,#23521,#23522,#23523,#23524,#23525,#23526,#23527,
#23528,#23529,#23530,#23531,#23532,#23533,#23534,#23535,#23536,#23537,#23538,
#23539,#23540,#23541,#23542,#23543,#23544,#23545,#23546,#23547,#23548,#23549,
#23550,#23551,#23552,#23553,#23554,#23555,#23556,#23557,#23558,#23559,#23560,
#23561,#23562,#23563,#23564,#23565,#23566,#23567,#23568,#23569,#23570,#23571,
#23572,#23573,#23574,#23575,#23576,#23577,#23578),.UNSPECIFIED.,.F.,.F.)
B_SPLINE_CURVE_WITH_KNOTS((6,1,1,1,1,1,1,1,1,1,1,1,1,1,1,1,1,1,1,1,1,1,
1,1,1,1,1,1,1,1,1,1,1,1,1,1,1,1,1,1,1,1,1,1,1,1,1,1,1,1,1,1,1,1,1,1,1,1,
1,1,1,1,1,1,1,6),(0.,0.0153846153846154,0.0307692307692308,0.0461538461538462,
0.0615384615384615,0.0769230769230769,0.0923076923076923,0.107692307692308,
0.123076923076923,0.138461538461538,0.153846153846154,0.169230769230769,
0.184615384615385,0.2,0.215384615384615,0.230769230769231,0.246153846153846,
0.261538461538462,0.276923076923077,0.292307692307692,0.307692307692308,
0.323076923076923,0.338461538461538,0.353846153846154,0.369230769230769,
0.384615384615385,0.4,0.415384615384615,0.430769230769231,0.446153846153846,
0.461538461538462,0.476923076923077,0.492307692307692,0.507692307692308,
0.523076923076923,0.538461538461538,0.553846153846154,0.569230769230769,
0.584615384615384,0.6,0.615384615384615,0.63076923076923,0.646153846153846,
0.661538461538461,0.676923076923076,0.692307692307692,0.707692307692307,
0.723076923076922,0.738461538461538,0.753846153846153,0.769230769230768,
0.784615384615384,0.799999999999999,0.815384615384614,0.83076923076923,
0.846153846153845,0.86153846153846,0.876923076923076,0.892307692307691,
0.907692307692306,0.923076923076922,0.938461538461537,0.953846153846152,
0.969230769230768,0.984615384615383,1.),.UNSPECIFIED.)
CURVE()
GEOMETRIC_REPRESENTATION_ITEM()
RATIONAL_B_SPLINE_CURVE((1.,1.,1.,1.,1.,1.,1.,1.,1.,1.,1.,1.,1.,1.,1.,1.,
1.,1.,1.,1.,1.,1.,1.,1.,1.,1.,1.,1.,1.,1.,1.,1.,1.,1.,1.,1.,1.,1.,1.,1.,
1.,1.,1.,1.,1.,1.,1.,1.,1.,1.,1.,1.,1.,1.,1.,1.,1.,1.,1.,1.,1.,1.,1.,1.,
1.,1.,1.,1.,1.,1.))
REPRESENTATION_ITEM('')
);
#61=(
BOUNDED_CURVE()
B_SPLINE_CURVE(5,(#23582,#23583,#23584,#23585,#23586,#23587,#23588,#23589,
#23590,#23591,#23592,#23593,#23594,#23595,#23596,#23597,#23598,#23599,#23600,
#23601,#23602,#23603,#23604,#23605,#23606,#23607,#23608,#23609,#23610,#23611,
#23612,#23613,#23614,#23615,#23616,#23617,#23618,#23619,#23620,#23621,#23622,
#23623,#23624,#23625,#23626,#23627,#23628,#23629,#23630,#23631,#23632,#23633,
#23634,#23635,#23636,#23637,#23638,#23639,#23640,#23641,#23642,#23643,#23644,
#23645,#23646,#23647,#23648,#23649,#23650,#23651),.UNSPECIFIED.,.F.,.F.)
B_SPLINE_CURVE_WITH_KNOTS((6,1,1,1,1,1,1,1,1,1,1,1,1,1,1,1,1,1,1,1,1,1,
1,1,1,1,1,1,1,1,1,1,1,1,1,1,1,1,1,1,1,1,1,1,1,1,1,1,1,1,1,1,1,1,1,1,1,1,
1,1,1,1,1,1,1,6),(0.,0.0153846153846154,0.0307692307692308,0.0461538461538462,
0.0615384615384615,0.0769230769230769,0.0923076923076923,0.107692307692308,
0.123076923076923,0.138461538461538,0.153846153846154,0.169230769230769,
0.184615384615385,0.2,0.215384615384615,0.230769230769231,0.246153846153846,
0.261538461538462,0.276923076923077,0.292307692307692,0.307692307692308,
0.323076923076923,0.338461538461538,0.353846153846154,0.369230769230769,
0.384615384615385,0.4,0.415384615384615,0.430769230769231,0.446153846153846,
0.461538461538462,0.476923076923077,0.492307692307692,0.507692307692308,
0.523076923076923,0.538461538461538,0.553846153846154,0.569230769230769,
0.584615384615384,0.6,0.615384615384615,0.63076923076923,0.646153846153846,
0.661538461538461,0.676923076923076,0.692307692307692,0.707692307692307,
0.723076923076922,0.738461538461538,0.753846153846153,0.769230769230768,
0.784615384615384,0.799999999999999,0.815384615384614,0.83076923076923,
0.846153846153845,0.86153846153846,0.876923076923076,0.892307692307691,
0.907692307692306,0.923076923076922,0.938461538461537,0.953846153846152,
0.969230769230768,0.984615384615383,1.),.UNSPECIFIED.)
CURVE()
GEOMETRIC_REPRESENTATION_ITEM()
RATIONAL_B_SPLINE_CURVE((1.,1.,1.,1.,1.,1.,1.,1.,1.,1.,1.,1.,1.,1.,1.,1.,
1.,1.,1.,1.,1.,1.,1.,1.,1.,1.,1.,1.,1.,1.,1.,1.,1.,1.,1.,1.,1.,1.,1.,1.,
1.,1.,1.,1.,1.,1.,1.,1.,1.,1.,1.,1.,1.,1.,1.,1.,1.,1.,1.,1.,1.,1.,1.,1.,
1.,1.,1.,1.,1.,1.))
REPRESENTATION_ITEM('')
);
#62=(
BOUNDED_CURVE()
B_SPLINE_CURVE(5,(#23655,#23656,#23657,#23658,#23659,#23660,#23661,#23662,
#23663,#23664,#23665,#23666,#23667,#23668,#23669,#23670,#23671,#23672,#23673,
#23674,#23675,#23676,#23677,#23678,#23679,#23680,#23681,#23682,#23683,#23684,
#23685,#23686,#23687,#23688,#23689,#23690,#23691,#23692,#23693,#23694,#23695,
#23696,#23697,#23698,#23699,#23700,#23701,#23702,#23703,#23704,#23705,#23706,
#23707,#23708,#23709,#23710,#23711,#23712,#23713,#23714,#23715,#23716,#23717,
#23718,#23719,#23720,#23721,#23722,#23723,#23724),.UNSPECIFIED.,.F.,.F.)
B_SPLINE_CURVE_WITH_KNOTS((6,1,1,1,1,1,1,1,1,1,1,1,1,1,1,1,1,1,1,1,1,1,
1,1,1,1,1,1,1,1,1,1,1,1,1,1,1,1,1,1,1,1,1,1,1,1,1,1,1,1,1,1,1,1,1,1,1,1,
1,1,1,1,1,1,1,6),(0.,0.0153846153846154,0.0307692307692308,0.0461538461538462,
0.0615384615384615,0.0769230769230769,0.0923076923076923,0.107692307692308,
0.123076923076923,0.138461538461538,0.153846153846154,0.169230769230769,
0.184615384615385,0.2,0.215384615384615,0.230769230769231,0.246153846153846,
0.261538461538462,0.276923076923077,0.292307692307692,0.307692307692308,
0.323076923076923,0.338461538461538,0.353846153846154,0.369230769230769,
0.384615384615385,0.4,0.415384615384615,0.430769230769231,0.446153846153846,
0.461538461538462,0.476923076923077,0.492307692307692,0.507692307692308,
0.523076923076923,0.538461538461538,0.553846153846154,0.569230769230769,
0.584615384615384,0.6,0.615384615384615,0.63076923076923,0.646153846153846,
0.661538461538461,0.676923076923076,0.692307692307692,0.707692307692307,
0.723076923076922,0.738461538461538,0.753846153846153,0.769230769230768,
0.784615384615384,0.799999999999999,0.815384615384614,0.83076923076923,
0.846153846153845,0.86153846153846,0.876923076923076,0.892307692307691,
0.907692307692306,0.923076923076922,0.938461538461537,0.953846153846152,
0.969230769230768,0.984615384615383,1.),.UNSPECIFIED.)
CURVE()
GEOMETRIC_REPRESENTATION_ITEM()
RATIONAL_B_SPLINE_CURVE((1.,1.,1.,1.,1.,1.,1.,1.,1.,1.,1.,1.,1.,1.,1.,1.,
1.,1.,1.,1.,1.,1.,1.,1.,1.,1.,1.,1.,1.,1.,1.,1.,1.,1.,1.,1.,1.,1.,1.,1.,
1.,1.,1.,1.,1.,1.,1.,1.,1.,1.,1.,1.,1.,1.,1.,1.,1.,1.,1.,1.,1.,1.,1.,1.,
1.,1.,1.,1.,1.,1.))
REPRESENTATION_ITEM('')
);
#63=(
BOUNDED_CURVE()
B_SPLINE_CURVE(5,(#23728,#23729,#23730,#23731,#23732,#23733,#23734,#23735,
#23736,#23737,#23738,#23739,#23740,#23741,#23742,#23743,#23744,#23745,#23746,
#23747,#23748,#23749,#23750,#23751,#23752,#23753,#23754,#23755,#23756,#23757,
#23758,#23759,#23760,#23761,#23762,#23763,#23764,#23765,#23766,#23767,#23768,
#23769,#23770,#23771,#23772,#23773,#23774,#23775,#23776,#23777,#23778,#23779,
#23780,#23781,#23782,#23783,#23784,#23785,#23786,#23787,#23788,#23789,#23790,
#23791,#23792,#23793,#23794,#23795,#23796,#23797),.UNSPECIFIED.,.F.,.F.)
B_SPLINE_CURVE_WITH_KNOTS((6,1,1,1,1,1,1,1,1,1,1,1,1,1,1,1,1,1,1,1,1,1,
1,1,1,1,1,1,1,1,1,1,1,1,1,1,1,1,1,1,1,1,1,1,1,1,1,1,1,1,1,1,1,1,1,1,1,1,
1,1,1,1,1,1,1,6),(0.,0.0153846153846154,0.0307692307692308,0.0461538461538462,
0.0615384615384615,0.0769230769230769,0.0923076923076923,0.107692307692308,
0.123076923076923,0.138461538461538,0.153846153846154,0.169230769230769,
0.184615384615385,0.2,0.215384615384615,0.230769230769231,0.246153846153846,
0.261538461538462,0.276923076923077,0.292307692307692,0.307692307692308,
0.323076923076923,0.338461538461538,0.353846153846154,0.369230769230769,
0.384615384615385,0.4,0.415384615384615,0.430769230769231,0.446153846153846,
0.461538461538462,0.476923076923077,0.492307692307692,0.507692307692308,
0.523076923076923,0.538461538461538,0.553846153846154,0.569230769230769,
0.584615384615384,0.6,0.615384615384615,0.63076923076923,0.646153846153846,
0.661538461538461,0.676923076923076,0.692307692307692,0.707692307692307,
0.723076923076922,0.738461538461538,0.753846153846153,0.769230769230768,
0.784615384615384,0.799999999999999,0.815384615384614,0.83076923076923,
0.846153846153845,0.86153846153846,0.876923076923076,0.892307692307691,
0.907692307692306,0.923076923076922,0.938461538461537,0.953846153846152,
0.969230769230768,0.984615384615383,1.),.UNSPECIFIED.)
CURVE()
GEOMETRIC_REPRESENTATION_ITEM()
RATIONAL_B_SPLINE_CURVE((1.,1.,1.,1.,1.,1.,1.,1.,1.,1.,1.,1.,1.,1.,1.,1.,
1.,1.,1.,1.,1.,1.,1.,1.,1.,1.,1.,1.,1.,1.,1.,1.,1.,1.,1.,1.,1.,1.,1.,1.,
1.,1.,1.,1.,1.,1.,1.,1.,1.,1.,1.,1.,1.,1.,1.,1.,1.,1.,1.,1.,1.,1.,1.,1.,
1.,1.,1.,1.,1.,1.))
REPRESENTATION_ITEM('')
);
#64=(
BOUNDED_CURVE()
B_SPLINE_CURVE(5,(#23801,#23802,#23803,#23804,#23805,#23806,#23807,#23808,
#23809,#23810,#23811,#23812,#23813,#23814,#23815,#23816,#23817,#23818,#23819,
#23820,#23821,#23822,#23823,#23824,#23825,#23826,#23827,#23828,#23829,#23830,
#23831,#23832,#23833,#23834,#23835,#23836,#23837,#23838,#23839,#23840,#23841,
#23842,#23843,#23844,#23845,#23846,#23847,#23848,#23849,#23850,#23851,#23852,
#23853,#23854,#23855,#23856,#23857,#23858,#23859,#23860,#23861,#23862,#23863,
#23864,#23865,#23866,#23867,#23868,#23869,#23870),.UNSPECIFIED.,.F.,.F.)
B_SPLINE_CURVE_WITH_KNOTS((6,1,1,1,1,1,1,1,1,1,1,1,1,1,1,1,1,1,1,1,1,1,
1,1,1,1,1,1,1,1,1,1,1,1,1,1,1,1,1,1,1,1,1,1,1,1,1,1,1,1,1,1,1,1,1,1,1,1,
1,1,1,1,1,1,1,6),(0.,0.0153846153846154,0.0307692307692308,0.0461538461538462,
0.0615384615384615,0.0769230769230769,0.0923076923076923,0.107692307692308,
0.123076923076923,0.138461538461538,0.153846153846154,0.169230769230769,
0.184615384615385,0.2,0.215384615384615,0.230769230769231,0.246153846153846,
0.261538461538462,0.276923076923077,0.292307692307692,0.307692307692308,
0.323076923076923,0.338461538461538,0.353846153846154,0.369230769230769,
0.384615384615385,0.4,0.415384615384615,0.430769230769231,0.446153846153846,
0.461538461538462,0.476923076923077,0.492307692307692,0.507692307692308,
0.523076923076923,0.538461538461538,0.553846153846154,0.569230769230769,
0.584615384615384,0.6,0.615384615384615,0.63076923076923,0.646153846153846,
0.661538461538461,0.676923076923076,0.692307692307692,0.707692307692307,
0.723076923076922,0.738461538461538,0.753846153846153,0.769230769230768,
0.784615384615384,0.799999999999999,0.815384615384614,0.83076923076923,
0.846153846153845,0.86153846153846,0.876923076923076,0.892307692307691,
0.907692307692306,0.923076923076922,0.938461538461537,0.953846153846152,
0.969230769230768,0.984615384615383,1.),.UNSPECIFIED.)
CURVE()
GEOMETRIC_REPRESENTATION_ITEM()
RATIONAL_B_SPLINE_CURVE((1.,1.,1.,1.,1.,1.,1.,1.,1.,1.,1.,1.,1.,1.,1.,1.,
1.,1.,1.,1.,1.,1.,1.,1.,1.,1.,1.,1.,1.,1.,1.,1.,1.,1.,1.,1.,1.,1.,1.,1.,
1.,1.,1.,1.,1.,1.,1.,1.,1.,1.,1.,1.,1.,1.,1.,1.,1.,1.,1.,1.,1.,1.,1.,1.,
1.,1.,1.,1.,1.,1.))
REPRESENTATION_ITEM('')
);
#65=(
BOUNDED_CURVE()
B_SPLINE_CURVE(5,(#23874,#23875,#23876,#23877,#23878,#23879,#23880,#23881,
#23882,#23883,#23884,#23885,#23886,#23887,#23888,#23889,#23890,#23891,#23892,
#23893,#23894,#23895,#23896,#23897,#23898,#23899,#23900,#23901,#23902,#23903,
#23904,#23905,#23906,#23907,#23908,#23909,#23910,#23911,#23912,#23913,#23914,
#23915,#23916,#23917,#23918,#23919,#23920,#23921,#23922,#23923,#23924,#23925,
#23926,#23927,#23928,#23929,#23930,#23931,#23932,#23933,#23934,#23935,#23936,
#23937,#23938,#23939,#23940,#23941,#23942,#23943),.UNSPECIFIED.,.F.,.F.)
B_SPLINE_CURVE_WITH_KNOTS((6,1,1,1,1,1,1,1,1,1,1,1,1,1,1,1,1,1,1,1,1,1,
1,1,1,1,1,1,1,1,1,1,1,1,1,1,1,1,1,1,1,1,1,1,1,1,1,1,1,1,1,1,1,1,1,1,1,1,
1,1,1,1,1,1,1,6),(0.,0.0153846153846154,0.0307692307692308,0.0461538461538462,
0.0615384615384615,0.0769230769230769,0.0923076923076923,0.107692307692308,
0.123076923076923,0.138461538461538,0.153846153846154,0.169230769230769,
0.184615384615385,0.2,0.215384615384615,0.230769230769231,0.246153846153846,
0.261538461538462,0.276923076923077,0.292307692307692,0.307692307692308,
0.323076923076923,0.338461538461538,0.353846153846154,0.369230769230769,
0.384615384615385,0.4,0.415384615384615,0.430769230769231,0.446153846153846,
0.461538461538462,0.476923076923077,0.492307692307692,0.507692307692308,
0.523076923076923,0.538461538461538,0.553846153846154,0.569230769230769,
0.584615384615384,0.6,0.615384615384615,0.63076923076923,0.646153846153846,
0.661538461538461,0.676923076923076,0.692307692307692,0.707692307692307,
0.723076923076922,0.738461538461538,0.753846153846153,0.769230769230768,
0.784615384615384,0.799999999999999,0.815384615384614,0.83076923076923,
0.846153846153845,0.86153846153846,0.876923076923076,0.892307692307691,
0.907692307692306,0.923076923076922,0.938461538461537,0.953846153846152,
0.969230769230768,0.984615384615383,1.),.UNSPECIFIED.)
CURVE()
GEOMETRIC_REPRESENTATION_ITEM()
RATIONAL_B_SPLINE_CURVE((1.,1.,1.,1.,1.,1.,1.,1.,1.,1.,1.,1.,1.,1.,1.,1.,
1.,1.,1.,1.,1.,1.,1.,1.,1.,1.,1.,1.,1.,1.,1.,1.,1.,1.,1.,1.,1.,1.,1.,1.,
1.,1.,1.,1.,1.,1.,1.,1.,1.,1.,1.,1.,1.,1.,1.,1.,1.,1.,1.,1.,1.,1.,1.,1.,
1.,1.,1.,1.,1.,1.))
REPRESENTATION_ITEM('')
);
#66=(
BOUNDED_CURVE()
B_SPLINE_CURVE(5,(#23947,#23948,#23949,#23950,#23951,#23952,#23953,#23954,
#23955,#23956,#23957,#23958,#23959,#23960,#23961,#23962,#23963,#23964,#23965,
#23966,#23967,#23968,#23969,#23970,#23971,#23972,#23973,#23974,#23975,#23976,
#23977,#23978,#23979,#23980,#23981,#23982,#23983,#23984,#23985,#23986,#23987,
#23988,#23989,#23990,#23991,#23992,#23993,#23994,#23995,#23996,#23997,#23998,
#23999,#24000,#24001,#24002,#24003,#24004,#24005,#24006,#24007,#24008,#24009,
#24010,#24011,#24012,#24013,#24014,#24015,#24016),.UNSPECIFIED.,.F.,.F.)
B_SPLINE_CURVE_WITH_KNOTS((6,1,1,1,1,1,1,1,1,1,1,1,1,1,1,1,1,1,1,1,1,1,
1,1,1,1,1,1,1,1,1,1,1,1,1,1,1,1,1,1,1,1,1,1,1,1,1,1,1,1,1,1,1,1,1,1,1,1,
1,1,1,1,1,1,1,6),(0.,0.0153846153846154,0.0307692307692308,0.0461538461538462,
0.0615384615384615,0.0769230769230769,0.0923076923076923,0.107692307692308,
0.123076923076923,0.138461538461538,0.153846153846154,0.169230769230769,
0.184615384615385,0.2,0.215384615384615,0.230769230769231,0.246153846153846,
0.261538461538462,0.276923076923077,0.292307692307692,0.307692307692308,
0.323076923076923,0.338461538461538,0.353846153846154,0.369230769230769,
0.384615384615385,0.4,0.415384615384615,0.430769230769231,0.446153846153846,
0.461538461538462,0.476923076923077,0.492307692307692,0.507692307692308,
0.523076923076923,0.538461538461538,0.553846153846154,0.569230769230769,
0.584615384615384,0.6,0.615384615384615,0.63076923076923,0.646153846153846,
0.661538461538461,0.676923076923076,0.692307692307692,0.707692307692307,
0.723076923076922,0.738461538461538,0.753846153846153,0.769230769230768,
0.784615384615384,0.799999999999999,0.815384615384614,0.83076923076923,
0.846153846153845,0.86153846153846,0.876923076923076,0.892307692307691,
0.907692307692306,0.923076923076922,0.938461538461537,0.953846153846152,
0.969230769230768,0.984615384615383,1.),.UNSPECIFIED.)
CURVE()
GEOMETRIC_REPRESENTATION_ITEM()
RATIONAL_B_SPLINE_CURVE((1.,1.,1.,1.,1.,1.,1.,1.,1.,1.,1.,1.,1.,1.,1.,1.,
1.,1.,1.,1.,1.,1.,1.,1.,1.,1.,1.,1.,1.,1.,1.,1.,1.,1.,1.,1.,1.,1.,1.,1.,
1.,1.,1.,1.,1.,1.,1.,1.,1.,1.,1.,1.,1.,1.,1.,1.,1.,1.,1.,1.,1.,1.,1.,1.,
1.,1.,1.,1.,1.,1.))
REPRESENTATION_ITEM('')
);
#67=(
BOUNDED_CURVE()
B_SPLINE_CURVE(5,(#24020,#24021,#24022,#24023,#24024,#24025,#24026,#24027,
#24028,#24029,#24030,#24031,#24032,#24033,#24034,#24035,#24036,#24037,#24038,
#24039,#24040,#24041,#24042,#24043,#24044,#24045,#24046,#24047,#24048,#24049,
#24050,#24051,#24052,#24053,#24054,#24055,#24056,#24057,#24058,#24059,#24060,
#24061,#24062,#24063,#24064,#24065,#24066,#24067,#24068,#24069,#24070,#24071,
#24072,#24073,#24074,#24075,#24076,#24077,#24078,#24079,#24080,#24081,#24082,
#24083,#24084,#24085,#24086,#24087,#24088,#24089),.UNSPECIFIED.,.F.,.F.)
B_SPLINE_CURVE_WITH_KNOTS((6,1,1,1,1,1,1,1,1,1,1,1,1,1,1,1,1,1,1,1,1,1,
1,1,1,1,1,1,1,1,1,1,1,1,1,1,1,1,1,1,1,1,1,1,1,1,1,1,1,1,1,1,1,1,1,1,1,1,
1,1,1,1,1,1,1,6),(0.,0.0153846153846154,0.0307692307692308,0.0461538461538462,
0.0615384615384615,0.0769230769230769,0.0923076923076923,0.107692307692308,
0.123076923076923,0.138461538461538,0.153846153846154,0.169230769230769,
0.184615384615385,0.2,0.215384615384615,0.230769230769231,0.246153846153846,
0.261538461538462,0.276923076923077,0.292307692307692,0.307692307692308,
0.323076923076923,0.338461538461538,0.353846153846154,0.369230769230769,
0.384615384615385,0.4,0.415384615384615,0.430769230769231,0.446153846153846,
0.461538461538462,0.476923076923077,0.492307692307692,0.507692307692308,
0.523076923076923,0.538461538461538,0.553846153846154,0.569230769230769,
0.584615384615384,0.6,0.615384615384615,0.63076923076923,0.646153846153846,
0.661538461538461,0.676923076923076,0.692307692307692,0.707692307692307,
0.723076923076922,0.738461538461538,0.753846153846153,0.769230769230768,
0.784615384615384,0.799999999999999,0.815384615384614,0.83076923076923,
0.846153846153845,0.86153846153846,0.876923076923076,0.892307692307691,
0.907692307692306,0.923076923076922,0.938461538461537,0.953846153846152,
0.969230769230768,0.984615384615383,1.),.UNSPECIFIED.)
CURVE()
GEOMETRIC_REPRESENTATION_ITEM()
RATIONAL_B_SPLINE_CURVE((1.,1.,1.,1.,1.,1.,1.,1.,1.,1.,1.,1.,1.,1.,1.,1.,
1.,1.,1.,1.,1.,1.,1.,1.,1.,1.,1.,1.,1.,1.,1.,1.,1.,1.,1.,1.,1.,1.,1.,1.,
1.,1.,1.,1.,1.,1.,1.,1.,1.,1.,1.,1.,1.,1.,1.,1.,1.,1.,1.,1.,1.,1.,1.,1.,
1.,1.,1.,1.,1.,1.))
REPRESENTATION_ITEM('')
);
#68=(
BOUNDED_CURVE()
B_SPLINE_CURVE(5,(#24093,#24094,#24095,#24096,#24097,#24098,#24099,#24100,
#24101,#24102,#24103,#24104,#24105,#24106,#24107,#24108,#24109,#24110,#24111,
#24112,#24113,#24114,#24115,#24116,#24117,#24118,#24119,#24120,#24121,#24122,
#24123,#24124,#24125,#24126,#24127,#24128,#24129,#24130,#24131,#24132,#24133,
#24134,#24135,#24136,#24137,#24138,#24139,#24140,#24141,#24142,#24143,#24144,
#24145,#24146,#24147,#24148,#24149,#24150,#24151,#24152,#24153,#24154,#24155,
#24156,#24157,#24158,#24159,#24160,#24161,#24162),.UNSPECIFIED.,.F.,.F.)
B_SPLINE_CURVE_WITH_KNOTS((6,1,1,1,1,1,1,1,1,1,1,1,1,1,1,1,1,1,1,1,1,1,
1,1,1,1,1,1,1,1,1,1,1,1,1,1,1,1,1,1,1,1,1,1,1,1,1,1,1,1,1,1,1,1,1,1,1,1,
1,1,1,1,1,1,1,6),(0.,0.0153846153846154,0.0307692307692308,0.0461538461538462,
0.0615384615384615,0.0769230769230769,0.0923076923076923,0.107692307692308,
0.123076923076923,0.138461538461538,0.153846153846154,0.169230769230769,
0.184615384615385,0.2,0.215384615384615,0.230769230769231,0.246153846153846,
0.261538461538462,0.276923076923077,0.292307692307692,0.307692307692308,
0.323076923076923,0.338461538461538,0.353846153846154,0.369230769230769,
0.384615384615385,0.4,0.415384615384615,0.430769230769231,0.446153846153846,
0.461538461538462,0.476923076923077,0.492307692307692,0.507692307692308,
0.523076923076923,0.538461538461538,0.553846153846154,0.569230769230769,
0.584615384615384,0.6,0.615384615384615,0.63076923076923,0.646153846153846,
0.661538461538461,0.676923076923076,0.692307692307692,0.707692307692307,
0.723076923076922,0.738461538461538,0.753846153846153,0.769230769230768,
0.784615384615384,0.799999999999999,0.815384615384614,0.83076923076923,
0.846153846153845,0.86153846153846,0.876923076923076,0.892307692307691,
0.907692307692306,0.923076923076922,0.938461538461537,0.953846153846152,
0.969230769230768,0.984615384615383,1.),.UNSPECIFIED.)
CURVE()
GEOMETRIC_REPRESENTATION_ITEM()
RATIONAL_B_SPLINE_CURVE((1.,1.,1.,1.,1.,1.,1.,1.,1.,1.,1.,1.,1.,1.,1.,1.,
1.,1.,1.,1.,1.,1.,1.,1.,1.,1.,1.,1.,1.,1.,1.,1.,1.,1.,1.,1.,1.,1.,1.,1.,
1.,1.,1.,1.,1.,1.,1.,1.,1.,1.,1.,1.,1.,1.,1.,1.,1.,1.,1.,1.,1.,1.,1.,1.,
1.,1.,1.,1.,1.,1.))
REPRESENTATION_ITEM('')
);
#69=(
BOUNDED_CURVE()
B_SPLINE_CURVE(5,(#24166,#24167,#24168,#24169,#24170,#24171,#24172,#24173,
#24174,#24175,#24176,#24177,#24178,#24179,#24180,#24181,#24182,#24183,#24184,
#24185,#24186,#24187,#24188,#24189,#24190,#24191,#24192,#24193,#24194,#24195,
#24196,#24197,#24198,#24199,#24200,#24201,#24202,#24203,#24204,#24205,#24206,
#24207,#24208,#24209,#24210,#24211,#24212,#24213,#24214,#24215,#24216,#24217,
#24218,#24219,#24220,#24221,#24222,#24223,#24224,#24225,#24226,#24227,#24228,
#24229,#24230,#24231,#24232,#24233,#24234,#24235),.UNSPECIFIED.,.F.,.F.)
B_SPLINE_CURVE_WITH_KNOTS((6,1,1,1,1,1,1,1,1,1,1,1,1,1,1,1,1,1,1,1,1,1,
1,1,1,1,1,1,1,1,1,1,1,1,1,1,1,1,1,1,1,1,1,1,1,1,1,1,1,1,1,1,1,1,1,1,1,1,
1,1,1,1,1,1,1,6),(0.,0.0153846153846154,0.0307692307692308,0.0461538461538462,
0.0615384615384615,0.0769230769230769,0.0923076923076923,0.107692307692308,
0.123076923076923,0.138461538461538,0.153846153846154,0.169230769230769,
0.184615384615385,0.2,0.215384615384615,0.230769230769231,0.246153846153846,
0.261538461538462,0.276923076923077,0.292307692307692,0.307692307692308,
0.323076923076923,0.338461538461538,0.353846153846154,0.369230769230769,
0.384615384615385,0.4,0.415384615384615,0.430769230769231,0.446153846153846,
0.461538461538462,0.476923076923077,0.492307692307692,0.507692307692308,
0.523076923076923,0.538461538461538,0.553846153846154,0.569230769230769,
0.584615384615384,0.6,0.615384615384615,0.63076923076923,0.646153846153846,
0.661538461538461,0.676923076923076,0.692307692307692,0.707692307692307,
0.723076923076922,0.738461538461538,0.753846153846153,0.769230769230768,
0.784615384615384,0.799999999999999,0.815384615384614,0.83076923076923,
0.846153846153845,0.86153846153846,0.876923076923076,0.892307692307691,
0.907692307692306,0.923076923076922,0.938461538461537,0.953846153846152,
0.969230769230768,0.984615384615383,1.),.UNSPECIFIED.)
CURVE()
GEOMETRIC_REPRESENTATION_ITEM()
RATIONAL_B_SPLINE_CURVE((1.,1.,1.,1.,1.,1.,1.,1.,1.,1.,1.,1.,1.,1.,1.,1.,
1.,1.,1.,1.,1.,1.,1.,1.,1.,1.,1.,1.,1.,1.,1.,1.,1.,1.,1.,1.,1.,1.,1.,1.,
1.,1.,1.,1.,1.,1.,1.,1.,1.,1.,1.,1.,1.,1.,1.,1.,1.,1.,1.,1.,1.,1.,1.,1.,
1.,1.,1.,1.,1.,1.))
REPRESENTATION_ITEM('')
);
#70=(
BOUNDED_CURVE()
B_SPLINE_CURVE(5,(#24239,#24240,#24241,#24242,#24243,#24244,#24245,#24246,
#24247,#24248,#24249,#24250,#24251,#24252,#24253,#24254,#24255,#24256,#24257,
#24258,#24259,#24260,#24261,#24262,#24263,#24264,#24265,#24266,#24267,#24268,
#24269,#24270,#24271,#24272,#24273,#24274,#24275,#24276,#24277,#24278,#24279,
#24280,#24281,#24282,#24283,#24284,#24285,#24286,#24287,#24288,#24289,#24290,
#24291,#24292,#24293,#24294,#24295,#24296,#24297,#24298,#24299,#24300,#24301,
#24302,#24303,#24304,#24305,#24306,#24307,#24308),.UNSPECIFIED.,.F.,.F.)
B_SPLINE_CURVE_WITH_KNOTS((6,1,1,1,1,1,1,1,1,1,1,1,1,1,1,1,1,1,1,1,1,1,
1,1,1,1,1,1,1,1,1,1,1,1,1,1,1,1,1,1,1,1,1,1,1,1,1,1,1,1,1,1,1,1,1,1,1,1,
1,1,1,1,1,1,1,6),(0.,0.0153846153846154,0.0307692307692308,0.0461538461538462,
0.0615384615384615,0.0769230769230769,0.0923076923076923,0.107692307692308,
0.123076923076923,0.138461538461538,0.153846153846154,0.169230769230769,
0.184615384615385,0.2,0.215384615384615,0.230769230769231,0.246153846153846,
0.261538461538462,0.276923076923077,0.292307692307692,0.307692307692308,
0.323076923076923,0.338461538461538,0.353846153846154,0.369230769230769,
0.384615384615385,0.4,0.415384615384615,0.430769230769231,0.446153846153846,
0.461538461538462,0.476923076923077,0.492307692307692,0.507692307692308,
0.523076923076923,0.538461538461538,0.553846153846154,0.569230769230769,
0.584615384615384,0.6,0.615384615384615,0.63076923076923,0.646153846153846,
0.661538461538461,0.676923076923076,0.692307692307692,0.707692307692307,
0.723076923076922,0.738461538461538,0.753846153846153,0.769230769230768,
0.784615384615384,0.799999999999999,0.815384615384614,0.83076923076923,
0.846153846153845,0.86153846153846,0.876923076923076,0.892307692307691,
0.907692307692306,0.923076923076922,0.938461538461537,0.953846153846152,
0.969230769230768,0.984615384615383,1.),.UNSPECIFIED.)
CURVE()
GEOMETRIC_REPRESENTATION_ITEM()
RATIONAL_B_SPLINE_CURVE((1.,1.,1.,1.,1.,1.,1.,1.,1.,1.,1.,1.,1.,1.,1.,1.,
1.,1.,1.,1.,1.,1.,1.,1.,1.,1.,1.,1.,1.,1.,1.,1.,1.,1.,1.,1.,1.,1.,1.,1.,
1.,1.,1.,1.,1.,1.,1.,1.,1.,1.,1.,1.,1.,1.,1.,1.,1.,1.,1.,1.,1.,1.,1.,1.,
1.,1.,1.,1.,1.,1.))
REPRESENTATION_ITEM('')
);
#71=(
BOUNDED_CURVE()
B_SPLINE_CURVE(5,(#24312,#24313,#24314,#24315,#24316,#24317,#24318,#24319,
#24320,#24321,#24322,#24323,#24324,#24325,#24326,#24327,#24328,#24329,#24330,
#24331,#24332,#24333,#24334,#24335,#24336,#24337,#24338,#24339,#24340,#24341,
#24342,#24343,#24344,#24345,#24346,#24347,#24348,#24349,#24350,#24351,#24352,
#24353,#24354,#24355,#24356,#24357,#24358,#24359,#24360,#24361,#24362,#24363,
#24364,#24365,#24366,#24367,#24368,#24369,#24370,#24371,#24372,#24373,#24374,
#24375,#24376,#24377,#24378,#24379,#24380,#24381),.UNSPECIFIED.,.F.,.F.)
B_SPLINE_CURVE_WITH_KNOTS((6,1,1,1,1,1,1,1,1,1,1,1,1,1,1,1,1,1,1,1,1,1,
1,1,1,1,1,1,1,1,1,1,1,1,1,1,1,1,1,1,1,1,1,1,1,1,1,1,1,1,1,1,1,1,1,1,1,1,
1,1,1,1,1,1,1,6),(0.,0.0153846153846154,0.0307692307692308,0.0461538461538462,
0.0615384615384615,0.0769230769230769,0.0923076923076923,0.107692307692308,
0.123076923076923,0.138461538461538,0.153846153846154,0.169230769230769,
0.184615384615385,0.2,0.215384615384615,0.230769230769231,0.246153846153846,
0.261538461538462,0.276923076923077,0.292307692307692,0.307692307692308,
0.323076923076923,0.338461538461538,0.353846153846154,0.369230769230769,
0.384615384615385,0.4,0.415384615384615,0.430769230769231,0.446153846153846,
0.461538461538462,0.476923076923077,0.492307692307692,0.507692307692308,
0.523076923076923,0.538461538461538,0.553846153846154,0.569230769230769,
0.584615384615384,0.6,0.615384615384615,0.63076923076923,0.646153846153846,
0.661538461538461,0.676923076923076,0.692307692307692,0.707692307692307,
0.723076923076922,0.738461538461538,0.753846153846153,0.769230769230768,
0.784615384615384,0.799999999999999,0.815384615384614,0.83076923076923,
0.846153846153845,0.86153846153846,0.876923076923076,0.892307692307691,
0.907692307692306,0.923076923076922,0.938461538461537,0.953846153846152,
0.969230769230768,0.984615384615383,1.),.UNSPECIFIED.)
CURVE()
GEOMETRIC_REPRESENTATION_ITEM()
RATIONAL_B_SPLINE_CURVE((1.,1.,1.,1.,1.,1.,1.,1.,1.,1.,1.,1.,1.,1.,1.,1.,
1.,1.,1.,1.,1.,1.,1.,1.,1.,1.,1.,1.,1.,1.,1.,1.,1.,1.,1.,1.,1.,1.,1.,1.,
1.,1.,1.,1.,1.,1.,1.,1.,1.,1.,1.,1.,1.,1.,1.,1.,1.,1.,1.,1.,1.,1.,1.,1.,
1.,1.,1.,1.,1.,1.))
REPRESENTATION_ITEM('')
);
#72=(
BOUNDED_CURVE()
B_SPLINE_CURVE(5,(#24385,#24386,#24387,#24388,#24389,#24390,#24391,#24392,
#24393,#24394,#24395,#24396,#24397,#24398,#24399,#24400,#24401,#24402,#24403,
#24404,#24405,#24406,#24407,#24408,#24409,#24410,#24411,#24412,#24413,#24414,
#24415,#24416,#24417,#24418,#24419,#24420,#24421,#24422,#24423,#24424,#24425,
#24426,#24427,#24428,#24429,#24430,#24431,#24432,#24433,#24434,#24435,#24436,
#24437,#24438,#24439,#24440,#24441,#24442,#24443,#24444,#24445,#24446,#24447,
#24448,#24449,#24450,#24451,#24452,#24453,#24454),.UNSPECIFIED.,.F.,.F.)
B_SPLINE_CURVE_WITH_KNOTS((6,1,1,1,1,1,1,1,1,1,1,1,1,1,1,1,1,1,1,1,1,1,
1,1,1,1,1,1,1,1,1,1,1,1,1,1,1,1,1,1,1,1,1,1,1,1,1,1,1,1,1,1,1,1,1,1,1,1,
1,1,1,1,1,1,1,6),(0.,0.0153846153846154,0.0307692307692308,0.0461538461538462,
0.0615384615384615,0.0769230769230769,0.0923076923076923,0.107692307692308,
0.123076923076923,0.138461538461538,0.153846153846154,0.169230769230769,
0.184615384615385,0.2,0.215384615384615,0.230769230769231,0.246153846153846,
0.261538461538462,0.276923076923077,0.292307692307692,0.307692307692308,
0.323076923076923,0.338461538461538,0.353846153846154,0.369230769230769,
0.384615384615385,0.4,0.415384615384615,0.430769230769231,0.446153846153846,
0.461538461538462,0.476923076923077,0.492307692307692,0.507692307692308,
0.523076923076923,0.538461538461538,0.553846153846154,0.569230769230769,
0.584615384615384,0.6,0.615384615384615,0.63076923076923,0.646153846153846,
0.661538461538461,0.676923076923076,0.692307692307692,0.707692307692307,
0.723076923076922,0.738461538461538,0.753846153846153,0.769230769230768,
0.784615384615384,0.799999999999999,0.815384615384614,0.83076923076923,
0.846153846153845,0.86153846153846,0.876923076923076,0.892307692307691,
0.907692307692306,0.923076923076922,0.938461538461537,0.953846153846152,
0.969230769230768,0.984615384615383,1.),.UNSPECIFIED.)
CURVE()
GEOMETRIC_REPRESENTATION_ITEM()
RATIONAL_B_SPLINE_CURVE((1.,1.,1.,1.,1.,1.,1.,1.,1.,1.,1.,1.,1.,1.,1.,1.,
1.,1.,1.,1.,1.,1.,1.,1.,1.,1.,1.,1.,1.,1.,1.,1.,1.,1.,1.,1.,1.,1.,1.,1.,
1.,1.,1.,1.,1.,1.,1.,1.,1.,1.,1.,1.,1.,1.,1.,1.,1.,1.,1.,1.,1.,1.,1.,1.,
1.,1.,1.,1.,1.,1.))
REPRESENTATION_ITEM('')
);
#73=(
BOUNDED_CURVE()
B_SPLINE_CURVE(5,(#24458,#24459,#24460,#24461,#24462,#24463,#24464,#24465,
#24466,#24467,#24468,#24469,#24470,#24471,#24472,#24473,#24474,#24475,#24476,
#24477,#24478,#24479,#24480,#24481,#24482,#24483,#24484,#24485,#24486,#24487,
#24488,#24489,#24490,#24491,#24492,#24493,#24494,#24495,#24496,#24497,#24498,
#24499,#24500,#24501,#24502,#24503,#24504,#24505,#24506,#24507,#24508,#24509,
#24510,#24511,#24512,#24513,#24514,#24515,#24516,#24517,#24518,#24519,#24520,
#24521,#24522,#24523,#24524,#24525,#24526,#24527),.UNSPECIFIED.,.F.,.F.)
B_SPLINE_CURVE_WITH_KNOTS((6,1,1,1,1,1,1,1,1,1,1,1,1,1,1,1,1,1,1,1,1,1,
1,1,1,1,1,1,1,1,1,1,1,1,1,1,1,1,1,1,1,1,1,1,1,1,1,1,1,1,1,1,1,1,1,1,1,1,
1,1,1,1,1,1,1,6),(0.,0.0153846153846154,0.0307692307692308,0.0461538461538462,
0.0615384615384615,0.0769230769230769,0.0923076923076923,0.107692307692308,
0.123076923076923,0.138461538461538,0.153846153846154,0.169230769230769,
0.184615384615385,0.2,0.215384615384615,0.230769230769231,0.246153846153846,
0.261538461538462,0.276923076923077,0.292307692307692,0.307692307692308,
0.323076923076923,0.338461538461538,0.353846153846154,0.369230769230769,
0.384615384615385,0.4,0.415384615384615,0.430769230769231,0.446153846153846,
0.461538461538462,0.476923076923077,0.492307692307692,0.507692307692308,
0.523076923076923,0.538461538461538,0.553846153846154,0.569230769230769,
0.584615384615384,0.6,0.615384615384615,0.63076923076923,0.646153846153846,
0.661538461538461,0.676923076923076,0.692307692307692,0.707692307692307,
0.723076923076922,0.738461538461538,0.753846153846153,0.769230769230768,
0.784615384615384,0.799999999999999,0.815384615384614,0.83076923076923,
0.846153846153845,0.86153846153846,0.876923076923076,0.892307692307691,
0.907692307692306,0.923076923076922,0.938461538461537,0.953846153846152,
0.969230769230768,0.984615384615383,1.),.UNSPECIFIED.)
CURVE()
GEOMETRIC_REPRESENTATION_ITEM()
RATIONAL_B_SPLINE_CURVE((1.,1.,1.,1.,1.,1.,1.,1.,1.,1.,1.,1.,1.,1.,1.,1.,
1.,1.,1.,1.,1.,1.,1.,1.,1.,1.,1.,1.,1.,1.,1.,1.,1.,1.,1.,1.,1.,1.,1.,1.,
1.,1.,1.,1.,1.,1.,1.,1.,1.,1.,1.,1.,1.,1.,1.,1.,1.,1.,1.,1.,1.,1.,1.,1.,
1.,1.,1.,1.,1.,1.))
REPRESENTATION_ITEM('')
);
#74=(
BOUNDED_CURVE()
B_SPLINE_CURVE(5,(#24531,#24532,#24533,#24534,#24535,#24536,#24537,#24538,
#24539,#24540,#24541,#24542,#24543,#24544,#24545,#24546,#24547,#24548,#24549,
#24550,#24551,#24552,#24553,#24554,#24555,#24556,#24557,#24558,#24559,#24560,
#24561,#24562,#24563,#24564,#24565,#24566,#24567,#24568,#24569,#24570,#24571,
#24572,#24573,#24574,#24575,#24576,#24577,#24578,#24579,#24580,#24581,#24582,
#24583,#24584,#24585,#24586,#24587,#24588,#24589,#24590,#24591,#24592,#24593,
#24594,#24595,#24596,#24597,#24598,#24599,#24600),.UNSPECIFIED.,.F.,.F.)
B_SPLINE_CURVE_WITH_KNOTS((6,1,1,1,1,1,1,1,1,1,1,1,1,1,1,1,1,1,1,1,1,1,
1,1,1,1,1,1,1,1,1,1,1,1,1,1,1,1,1,1,1,1,1,1,1,1,1,1,1,1,1,1,1,1,1,1,1,1,
1,1,1,1,1,1,1,6),(0.,0.0153846153846154,0.0307692307692308,0.0461538461538462,
0.0615384615384615,0.0769230769230769,0.0923076923076923,0.107692307692308,
0.123076923076923,0.138461538461538,0.153846153846154,0.169230769230769,
0.184615384615385,0.2,0.215384615384615,0.230769230769231,0.246153846153846,
0.261538461538462,0.276923076923077,0.292307692307692,0.307692307692308,
0.323076923076923,0.338461538461538,0.353846153846154,0.369230769230769,
0.384615384615385,0.4,0.415384615384615,0.430769230769231,0.446153846153846,
0.461538461538462,0.476923076923077,0.492307692307692,0.507692307692308,
0.523076923076923,0.538461538461538,0.553846153846154,0.569230769230769,
0.584615384615384,0.6,0.615384615384615,0.63076923076923,0.646153846153846,
0.661538461538461,0.676923076923076,0.692307692307692,0.707692307692307,
0.723076923076922,0.738461538461538,0.753846153846153,0.769230769230768,
0.784615384615384,0.799999999999999,0.815384615384614,0.83076923076923,
0.846153846153845,0.86153846153846,0.876923076923076,0.892307692307691,
0.907692307692306,0.923076923076922,0.938461538461537,0.953846153846152,
0.969230769230768,0.984615384615383,1.),.UNSPECIFIED.)
CURVE()
GEOMETRIC_REPRESENTATION_ITEM()
RATIONAL_B_SPLINE_CURVE((1.,1.,1.,1.,1.,1.,1.,1.,1.,1.,1.,1.,1.,1.,1.,1.,
1.,1.,1.,1.,1.,1.,1.,1.,1.,1.,1.,1.,1.,1.,1.,1.,1.,1.,1.,1.,1.,1.,1.,1.,
1.,1.,1.,1.,1.,1.,1.,1.,1.,1.,1.,1.,1.,1.,1.,1.,1.,1.,1.,1.,1.,1.,1.,1.,
1.,1.,1.,1.,1.,1.))
REPRESENTATION_ITEM('')
);
#75=(
BOUNDED_CURVE()
B_SPLINE_CURVE(5,(#24604,#24605,#24606,#24607,#24608,#24609,#24610,#24611,
#24612,#24613,#24614,#24615,#24616,#24617,#24618,#24619,#24620,#24621,#24622,
#24623,#24624,#24625,#24626,#24627,#24628,#24629,#24630,#24631,#24632,#24633,
#24634,#24635,#24636,#24637,#24638,#24639,#24640,#24641,#24642,#24643,#24644,
#24645,#24646,#24647,#24648,#24649,#24650,#24651,#24652,#24653,#24654,#24655,
#24656,#24657,#24658,#24659,#24660,#24661,#24662,#24663,#24664,#24665,#24666,
#24667,#24668,#24669,#24670,#24671,#24672,#24673),.UNSPECIFIED.,.F.,.F.)
B_SPLINE_CURVE_WITH_KNOTS((6,1,1,1,1,1,1,1,1,1,1,1,1,1,1,1,1,1,1,1,1,1,
1,1,1,1,1,1,1,1,1,1,1,1,1,1,1,1,1,1,1,1,1,1,1,1,1,1,1,1,1,1,1,1,1,1,1,1,
1,1,1,1,1,1,1,6),(0.,0.0153846153846154,0.0307692307692308,0.0461538461538462,
0.0615384615384615,0.0769230769230769,0.0923076923076923,0.107692307692308,
0.123076923076923,0.138461538461538,0.153846153846154,0.169230769230769,
0.184615384615385,0.2,0.215384615384615,0.230769230769231,0.246153846153846,
0.261538461538462,0.276923076923077,0.292307692307692,0.307692307692308,
0.323076923076923,0.338461538461538,0.353846153846154,0.369230769230769,
0.384615384615385,0.4,0.415384615384615,0.430769230769231,0.446153846153846,
0.461538461538462,0.476923076923077,0.492307692307692,0.507692307692308,
0.523076923076923,0.538461538461538,0.553846153846154,0.569230769230769,
0.584615384615384,0.6,0.615384615384615,0.63076923076923,0.646153846153846,
0.661538461538461,0.676923076923076,0.692307692307692,0.707692307692307,
0.723076923076922,0.738461538461538,0.753846153846153,0.769230769230768,
0.784615384615384,0.799999999999999,0.815384615384614,0.83076923076923,
0.846153846153845,0.86153846153846,0.876923076923076,0.892307692307691,
0.907692307692306,0.923076923076922,0.938461538461537,0.953846153846152,
0.969230769230768,0.984615384615383,1.),.UNSPECIFIED.)
CURVE()
GEOMETRIC_REPRESENTATION_ITEM()
RATIONAL_B_SPLINE_CURVE((1.,1.,1.,1.,1.,1.,1.,1.,1.,1.,1.,1.,1.,1.,1.,1.,
1.,1.,1.,1.,1.,1.,1.,1.,1.,1.,1.,1.,1.,1.,1.,1.,1.,1.,1.,1.,1.,1.,1.,1.,
1.,1.,1.,1.,1.,1.,1.,1.,1.,1.,1.,1.,1.,1.,1.,1.,1.,1.,1.,1.,1.,1.,1.,1.,
1.,1.,1.,1.,1.,1.))
REPRESENTATION_ITEM('')
);
#76=(
BOUNDED_CURVE()
B_SPLINE_CURVE(5,(#24677,#24678,#24679,#24680,#24681,#24682,#24683,#24684,
#24685,#24686,#24687,#24688,#24689,#24690,#24691,#24692,#24693,#24694,#24695,
#24696,#24697,#24698,#24699,#24700,#24701,#24702,#24703,#24704,#24705,#24706,
#24707,#24708,#24709,#24710,#24711,#24712,#24713,#24714,#24715,#24716,#24717,
#24718,#24719,#24720,#24721,#24722,#24723,#24724,#24725,#24726,#24727,#24728,
#24729,#24730,#24731,#24732,#24733,#24734,#24735,#24736,#24737,#24738,#24739,
#24740,#24741,#24742,#24743,#24744,#24745,#24746),.UNSPECIFIED.,.F.,.F.)
B_SPLINE_CURVE_WITH_KNOTS((6,1,1,1,1,1,1,1,1,1,1,1,1,1,1,1,1,1,1,1,1,1,
1,1,1,1,1,1,1,1,1,1,1,1,1,1,1,1,1,1,1,1,1,1,1,1,1,1,1,1,1,1,1,1,1,1,1,1,
1,1,1,1,1,1,1,6),(0.,0.0153846153846154,0.0307692307692308,0.0461538461538462,
0.0615384615384615,0.0769230769230769,0.0923076923076923,0.107692307692308,
0.123076923076923,0.138461538461538,0.153846153846154,0.169230769230769,
0.184615384615385,0.2,0.215384615384615,0.230769230769231,0.246153846153846,
0.261538461538462,0.276923076923077,0.292307692307692,0.307692307692308,
0.323076923076923,0.338461538461538,0.353846153846154,0.369230769230769,
0.384615384615385,0.4,0.415384615384615,0.430769230769231,0.446153846153846,
0.461538461538462,0.476923076923077,0.492307692307692,0.507692307692308,
0.523076923076923,0.538461538461538,0.553846153846154,0.569230769230769,
0.584615384615384,0.6,0.615384615384615,0.63076923076923,0.646153846153846,
0.661538461538461,0.676923076923076,0.692307692307692,0.707692307692307,
0.723076923076922,0.738461538461538,0.753846153846153,0.769230769230768,
0.784615384615384,0.799999999999999,0.815384615384614,0.83076923076923,
0.846153846153845,0.86153846153846,0.876923076923076,0.892307692307691,
0.907692307692306,0.923076923076922,0.938461538461537,0.953846153846152,
0.969230769230768,0.984615384615383,1.),.UNSPECIFIED.)
CURVE()
GEOMETRIC_REPRESENTATION_ITEM()
RATIONAL_B_SPLINE_CURVE((1.,1.,1.,1.,1.,1.,1.,1.,1.,1.,1.,1.,1.,1.,1.,1.,
1.,1.,1.,1.,1.,1.,1.,1.,1.,1.,1.,1.,1.,1.,1.,1.,1.,1.,1.,1.,1.,1.,1.,1.,
1.,1.,1.,1.,1.,1.,1.,1.,1.,1.,1.,1.,1.,1.,1.,1.,1.,1.,1.,1.,1.,1.,1.,1.,
1.,1.,1.,1.,1.,1.))
REPRESENTATION_ITEM('')
);
#77=(
BOUNDED_CURVE()
B_SPLINE_CURVE(5,(#24750,#24751,#24752,#24753,#24754,#24755,#24756,#24757,
#24758,#24759,#24760,#24761,#24762,#24763,#24764,#24765,#24766,#24767,#24768,
#24769,#24770,#24771,#24772,#24773,#24774,#24775,#24776,#24777,#24778,#24779,
#24780,#24781,#24782,#24783,#24784,#24785,#24786,#24787,#24788,#24789,#24790,
#24791,#24792,#24793,#24794,#24795,#24796,#24797,#24798,#24799,#24800,#24801,
#24802,#24803,#24804,#24805,#24806,#24807,#24808,#24809,#24810,#24811,#24812,
#24813,#24814,#24815,#24816,#24817,#24818,#24819),.UNSPECIFIED.,.F.,.F.)
B_SPLINE_CURVE_WITH_KNOTS((6,1,1,1,1,1,1,1,1,1,1,1,1,1,1,1,1,1,1,1,1,1,
1,1,1,1,1,1,1,1,1,1,1,1,1,1,1,1,1,1,1,1,1,1,1,1,1,1,1,1,1,1,1,1,1,1,1,1,
1,1,1,1,1,1,1,6),(0.,0.0153846153846154,0.0307692307692308,0.0461538461538462,
0.0615384615384615,0.0769230769230769,0.0923076923076923,0.107692307692308,
0.123076923076923,0.138461538461538,0.153846153846154,0.169230769230769,
0.184615384615385,0.2,0.215384615384615,0.230769230769231,0.246153846153846,
0.261538461538462,0.276923076923077,0.292307692307692,0.307692307692308,
0.323076923076923,0.338461538461538,0.353846153846154,0.369230769230769,
0.384615384615385,0.4,0.415384615384615,0.430769230769231,0.446153846153846,
0.461538461538462,0.476923076923077,0.492307692307692,0.507692307692308,
0.523076923076923,0.538461538461538,0.553846153846154,0.569230769230769,
0.584615384615384,0.6,0.615384615384615,0.63076923076923,0.646153846153846,
0.661538461538461,0.676923076923076,0.692307692307692,0.707692307692307,
0.723076923076922,0.738461538461538,0.753846153846153,0.769230769230768,
0.784615384615384,0.799999999999999,0.815384615384614,0.83076923076923,
0.846153846153845,0.86153846153846,0.876923076923076,0.892307692307691,
0.907692307692306,0.923076923076922,0.938461538461537,0.953846153846152,
0.969230769230768,0.984615384615383,1.),.UNSPECIFIED.)
CURVE()
GEOMETRIC_REPRESENTATION_ITEM()
RATIONAL_B_SPLINE_CURVE((1.,1.,1.,1.,1.,1.,1.,1.,1.,1.,1.,1.,1.,1.,1.,1.,
1.,1.,1.,1.,1.,1.,1.,1.,1.,1.,1.,1.,1.,1.,1.,1.,1.,1.,1.,1.,1.,1.,1.,1.,
1.,1.,1.,1.,1.,1.,1.,1.,1.,1.,1.,1.,1.,1.,1.,1.,1.,1.,1.,1.,1.,1.,1.,1.,
1.,1.,1.,1.,1.,1.))
REPRESENTATION_ITEM('')
);
#78=(
BOUNDED_CURVE()
B_SPLINE_CURVE(5,(#24823,#24824,#24825,#24826,#24827,#24828,#24829,#24830,
#24831,#24832,#24833,#24834,#24835,#24836,#24837,#24838,#24839,#24840,#24841,
#24842,#24843,#24844,#24845,#24846,#24847,#24848,#24849,#24850,#24851,#24852,
#24853,#24854,#24855,#24856,#24857,#24858,#24859,#24860,#24861,#24862,#24863,
#24864,#24865,#24866,#24867,#24868,#24869,#24870,#24871,#24872,#24873,#24874,
#24875,#24876,#24877,#24878,#24879,#24880,#24881,#24882,#24883,#24884,#24885,
#24886,#24887,#24888,#24889,#24890,#24891,#24892),.UNSPECIFIED.,.F.,.F.)
B_SPLINE_CURVE_WITH_KNOTS((6,1,1,1,1,1,1,1,1,1,1,1,1,1,1,1,1,1,1,1,1,1,
1,1,1,1,1,1,1,1,1,1,1,1,1,1,1,1,1,1,1,1,1,1,1,1,1,1,1,1,1,1,1,1,1,1,1,1,
1,1,1,1,1,1,1,6),(0.,0.0153846153846154,0.0307692307692308,0.0461538461538462,
0.0615384615384615,0.0769230769230769,0.0923076923076923,0.107692307692308,
0.123076923076923,0.138461538461538,0.153846153846154,0.169230769230769,
0.184615384615385,0.2,0.215384615384615,0.230769230769231,0.246153846153846,
0.261538461538462,0.276923076923077,0.292307692307692,0.307692307692308,
0.323076923076923,0.338461538461538,0.353846153846154,0.369230769230769,
0.384615384615385,0.4,0.415384615384615,0.430769230769231,0.446153846153846,
0.461538461538462,0.476923076923077,0.492307692307692,0.507692307692308,
0.523076923076923,0.538461538461538,0.553846153846154,0.569230769230769,
0.584615384615384,0.6,0.615384615384615,0.63076923076923,0.646153846153846,
0.661538461538461,0.676923076923076,0.692307692307692,0.707692307692307,
0.723076923076922,0.738461538461538,0.753846153846153,0.769230769230768,
0.784615384615384,0.799999999999999,0.815384615384614,0.83076923076923,
0.846153846153845,0.86153846153846,0.876923076923076,0.892307692307691,
0.907692307692306,0.923076923076922,0.938461538461537,0.953846153846152,
0.969230769230768,0.984615384615383,1.),.UNSPECIFIED.)
CURVE()
GEOMETRIC_REPRESENTATION_ITEM()
RATIONAL_B_SPLINE_CURVE((1.,1.,1.,1.,1.,1.,1.,1.,1.,1.,1.,1.,1.,1.,1.,1.,
1.,1.,1.,1.,1.,1.,1.,1.,1.,1.,1.,1.,1.,1.,1.,1.,1.,1.,1.,1.,1.,1.,1.,1.,
1.,1.,1.,1.,1.,1.,1.,1.,1.,1.,1.,1.,1.,1.,1.,1.,1.,1.,1.,1.,1.,1.,1.,1.,
1.,1.,1.,1.,1.,1.))
REPRESENTATION_ITEM('')
);
#79=(
BOUNDED_CURVE()
B_SPLINE_CURVE(5,(#24896,#24897,#24898,#24899,#24900,#24901,#24902,#24903,
#24904,#24905,#24906,#24907,#24908,#24909,#24910,#24911,#24912,#24913,#24914,
#24915,#24916,#24917,#24918,#24919,#24920,#24921,#24922,#24923,#24924,#24925,
#24926,#24927,#24928,#24929,#24930,#24931,#24932,#24933,#24934,#24935,#24936,
#24937,#24938,#24939,#24940,#24941,#24942,#24943,#24944,#24945,#24946,#24947,
#24948,#24949,#24950,#24951,#24952,#24953,#24954,#24955,#24956,#24957,#24958,
#24959,#24960,#24961,#24962,#24963,#24964,#24965),.UNSPECIFIED.,.F.,.F.)
B_SPLINE_CURVE_WITH_KNOTS((6,1,1,1,1,1,1,1,1,1,1,1,1,1,1,1,1,1,1,1,1,1,
1,1,1,1,1,1,1,1,1,1,1,1,1,1,1,1,1,1,1,1,1,1,1,1,1,1,1,1,1,1,1,1,1,1,1,1,
1,1,1,1,1,1,1,6),(0.,0.0153846153846154,0.0307692307692308,0.0461538461538462,
0.0615384615384615,0.0769230769230769,0.0923076923076923,0.107692307692308,
0.123076923076923,0.138461538461538,0.153846153846154,0.169230769230769,
0.184615384615385,0.2,0.215384615384615,0.230769230769231,0.246153846153846,
0.261538461538462,0.276923076923077,0.292307692307692,0.307692307692308,
0.323076923076923,0.338461538461538,0.353846153846154,0.369230769230769,
0.384615384615385,0.4,0.415384615384615,0.430769230769231,0.446153846153846,
0.461538461538462,0.476923076923077,0.492307692307692,0.507692307692308,
0.523076923076923,0.538461538461538,0.553846153846154,0.569230769230769,
0.584615384615384,0.6,0.615384615384615,0.63076923076923,0.646153846153846,
0.661538461538461,0.676923076923076,0.692307692307692,0.707692307692307,
0.723076923076922,0.738461538461538,0.753846153846153,0.769230769230768,
0.784615384615384,0.799999999999999,0.815384615384614,0.83076923076923,
0.846153846153845,0.86153846153846,0.876923076923076,0.892307692307691,
0.907692307692306,0.923076923076922,0.938461538461537,0.953846153846152,
0.969230769230768,0.984615384615383,1.),.UNSPECIFIED.)
CURVE()
GEOMETRIC_REPRESENTATION_ITEM()
RATIONAL_B_SPLINE_CURVE((1.,1.,1.,1.,1.,1.,1.,1.,1.,1.,1.,1.,1.,1.,1.,1.,
1.,1.,1.,1.,1.,1.,1.,1.,1.,1.,1.,1.,1.,1.,1.,1.,1.,1.,1.,1.,1.,1.,1.,1.,
1.,1.,1.,1.,1.,1.,1.,1.,1.,1.,1.,1.,1.,1.,1.,1.,1.,1.,1.,1.,1.,1.,1.,1.,
1.,1.,1.,1.,1.,1.))
REPRESENTATION_ITEM('')
);
#80=(
BOUNDED_CURVE()
B_SPLINE_CURVE(5,(#24969,#24970,#24971,#24972,#24973,#24974,#24975,#24976,
#24977,#24978,#24979,#24980,#24981,#24982,#24983,#24984,#24985,#24986,#24987,
#24988,#24989,#24990,#24991,#24992,#24993,#24994,#24995,#24996,#24997,#24998,
#24999,#25000,#25001,#25002,#25003,#25004,#25005,#25006,#25007,#25008,#25009,
#25010,#25011,#25012,#25013,#25014,#25015,#25016,#25017,#25018,#25019,#25020,
#25021,#25022,#25023,#25024,#25025,#25026,#25027,#25028,#25029,#25030,#25031,
#25032,#25033,#25034,#25035,#25036,#25037,#25038),.UNSPECIFIED.,.F.,.F.)
B_SPLINE_CURVE_WITH_KNOTS((6,1,1,1,1,1,1,1,1,1,1,1,1,1,1,1,1,1,1,1,1,1,
1,1,1,1,1,1,1,1,1,1,1,1,1,1,1,1,1,1,1,1,1,1,1,1,1,1,1,1,1,1,1,1,1,1,1,1,
1,1,1,1,1,1,1,6),(0.,0.0153846153846154,0.0307692307692308,0.0461538461538462,
0.0615384615384615,0.0769230769230769,0.0923076923076923,0.107692307692308,
0.123076923076923,0.138461538461538,0.153846153846154,0.169230769230769,
0.184615384615385,0.2,0.215384615384615,0.230769230769231,0.246153846153846,
0.261538461538462,0.276923076923077,0.292307692307692,0.307692307692308,
0.323076923076923,0.338461538461538,0.353846153846154,0.369230769230769,
0.384615384615385,0.4,0.415384615384615,0.430769230769231,0.446153846153846,
0.461538461538462,0.476923076923077,0.492307692307692,0.507692307692308,
0.523076923076923,0.538461538461538,0.553846153846154,0.569230769230769,
0.584615384615384,0.6,0.615384615384615,0.63076923076923,0.646153846153846,
0.661538461538461,0.676923076923076,0.692307692307692,0.707692307692307,
0.723076923076922,0.738461538461538,0.753846153846153,0.769230769230768,
0.784615384615384,0.799999999999999,0.815384615384614,0.83076923076923,
0.846153846153845,0.86153846153846,0.876923076923076,0.892307692307691,
0.907692307692306,0.923076923076922,0.938461538461537,0.953846153846152,
0.969230769230768,0.984615384615383,1.),.UNSPECIFIED.)
CURVE()
GEOMETRIC_REPRESENTATION_ITEM()
RATIONAL_B_SPLINE_CURVE((1.,1.,1.,1.,1.,1.,1.,1.,1.,1.,1.,1.,1.,1.,1.,1.,
1.,1.,1.,1.,1.,1.,1.,1.,1.,1.,1.,1.,1.,1.,1.,1.,1.,1.,1.,1.,1.,1.,1.,1.,
1.,1.,1.,1.,1.,1.,1.,1.,1.,1.,1.,1.,1.,1.,1.,1.,1.,1.,1.,1.,1.,1.,1.,1.,
1.,1.,1.,1.,1.,1.))
REPRESENTATION_ITEM('')
);
#81=(
BOUNDED_CURVE()
B_SPLINE_CURVE(5,(#25042,#25043,#25044,#25045,#25046,#25047,#25048,#25049,
#25050,#25051,#25052,#25053,#25054,#25055,#25056,#25057,#25058,#25059,#25060,
#25061,#25062,#25063,#25064,#25065,#25066,#25067,#25068,#25069,#25070,#25071,
#25072,#25073,#25074,#25075,#25076,#25077,#25078,#25079,#25080,#25081,#25082,
#25083,#25084,#25085,#25086,#25087,#25088,#25089,#25090,#25091,#25092,#25093,
#25094,#25095,#25096,#25097,#25098,#25099,#25100,#25101,#25102,#25103,#25104,
#25105,#25106,#25107,#25108,#25109,#25110,#25111),.UNSPECIFIED.,.F.,.F.)
B_SPLINE_CURVE_WITH_KNOTS((6,1,1,1,1,1,1,1,1,1,1,1,1,1,1,1,1,1,1,1,1,1,
1,1,1,1,1,1,1,1,1,1,1,1,1,1,1,1,1,1,1,1,1,1,1,1,1,1,1,1,1,1,1,1,1,1,1,1,
1,1,1,1,1,1,1,6),(0.,0.0153846153846154,0.0307692307692308,0.0461538461538462,
0.0615384615384615,0.0769230769230769,0.0923076923076923,0.107692307692308,
0.123076923076923,0.138461538461538,0.153846153846154,0.169230769230769,
0.184615384615385,0.2,0.215384615384615,0.230769230769231,0.246153846153846,
0.261538461538462,0.276923076923077,0.292307692307692,0.307692307692308,
0.323076923076923,0.338461538461538,0.353846153846154,0.369230769230769,
0.384615384615385,0.4,0.415384615384615,0.430769230769231,0.446153846153846,
0.461538461538462,0.476923076923077,0.492307692307692,0.507692307692308,
0.523076923076923,0.538461538461538,0.553846153846154,0.569230769230769,
0.584615384615384,0.6,0.615384615384615,0.63076923076923,0.646153846153846,
0.661538461538461,0.676923076923076,0.692307692307692,0.707692307692307,
0.723076923076922,0.738461538461538,0.753846153846153,0.769230769230768,
0.784615384615384,0.799999999999999,0.815384615384614,0.83076923076923,
0.846153846153845,0.86153846153846,0.876923076923076,0.892307692307691,
0.907692307692306,0.923076923076922,0.938461538461537,0.953846153846152,
0.969230769230768,0.984615384615383,1.),.UNSPECIFIED.)
CURVE()
GEOMETRIC_REPRESENTATION_ITEM()
RATIONAL_B_SPLINE_CURVE((1.,1.,1.,1.,1.,1.,1.,1.,1.,1.,1.,1.,1.,1.,1.,1.,
1.,1.,1.,1.,1.,1.,1.,1.,1.,1.,1.,1.,1.,1.,1.,1.,1.,1.,1.,1.,1.,1.,1.,1.,
1.,1.,1.,1.,1.,1.,1.,1.,1.,1.,1.,1.,1.,1.,1.,1.,1.,1.,1.,1.,1.,1.,1.,1.,
1.,1.,1.,1.,1.,1.))
REPRESENTATION_ITEM('')
);
#82=(
BOUNDED_CURVE()
B_SPLINE_CURVE(5,(#25115,#25116,#25117,#25118,#25119,#25120,#25121,#25122,
#25123,#25124,#25125,#25126,#25127,#25128,#25129,#25130,#25131,#25132,#25133,
#25134,#25135,#25136,#25137,#25138,#25139,#25140,#25141,#25142,#25143,#25144,
#25145,#25146,#25147,#25148,#25149,#25150,#25151,#25152,#25153,#25154,#25155,
#25156,#25157,#25158,#25159,#25160,#25161,#25162,#25163,#25164,#25165,#25166,
#25167,#25168,#25169,#25170,#25171,#25172,#25173,#25174,#25175,#25176,#25177,
#25178,#25179,#25180,#25181,#25182,#25183,#25184),.UNSPECIFIED.,.F.,.F.)
B_SPLINE_CURVE_WITH_KNOTS((6,1,1,1,1,1,1,1,1,1,1,1,1,1,1,1,1,1,1,1,1,1,
1,1,1,1,1,1,1,1,1,1,1,1,1,1,1,1,1,1,1,1,1,1,1,1,1,1,1,1,1,1,1,1,1,1,1,1,
1,1,1,1,1,1,1,6),(0.,0.0153846153846154,0.0307692307692308,0.0461538461538462,
0.0615384615384615,0.0769230769230769,0.0923076923076923,0.107692307692308,
0.123076923076923,0.138461538461538,0.153846153846154,0.169230769230769,
0.184615384615385,0.2,0.215384615384615,0.230769230769231,0.246153846153846,
0.261538461538462,0.276923076923077,0.292307692307692,0.307692307692308,
0.323076923076923,0.338461538461538,0.353846153846154,0.369230769230769,
0.384615384615385,0.4,0.415384615384615,0.430769230769231,0.446153846153846,
0.461538461538462,0.476923076923077,0.492307692307692,0.507692307692308,
0.523076923076923,0.538461538461538,0.553846153846154,0.569230769230769,
0.584615384615384,0.6,0.615384615384615,0.63076923076923,0.646153846153846,
0.661538461538461,0.676923076923076,0.692307692307692,0.707692307692307,
0.723076923076922,0.738461538461538,0.753846153846153,0.769230769230768,
0.784615384615384,0.799999999999999,0.815384615384614,0.83076923076923,
0.846153846153845,0.86153846153846,0.876923076923076,0.892307692307691,
0.907692307692306,0.923076923076922,0.938461538461537,0.953846153846152,
0.969230769230768,0.984615384615383,1.),.UNSPECIFIED.)
CURVE()
GEOMETRIC_REPRESENTATION_ITEM()
RATIONAL_B_SPLINE_CURVE((1.,1.,1.,1.,1.,1.,1.,1.,1.,1.,1.,1.,1.,1.,1.,1.,
1.,1.,1.,1.,1.,1.,1.,1.,1.,1.,1.,1.,1.,1.,1.,1.,1.,1.,1.,1.,1.,1.,1.,1.,
1.,1.,1.,1.,1.,1.,1.,1.,1.,1.,1.,1.,1.,1.,1.,1.,1.,1.,1.,1.,1.,1.,1.,1.,
1.,1.,1.,1.,1.,1.))
REPRESENTATION_ITEM('')
);
#83=(
BOUNDED_CURVE()
B_SPLINE_CURVE(5,(#25188,#25189,#25190,#25191,#25192,#25193,#25194,#25195,
#25196,#25197,#25198,#25199,#25200,#25201,#25202,#25203,#25204,#25205,#25206,
#25207,#25208,#25209,#25210,#25211,#25212,#25213,#25214,#25215,#25216,#25217,
#25218,#25219,#25220,#25221,#25222,#25223,#25224,#25225,#25226,#25227,#25228,
#25229,#25230,#25231,#25232,#25233,#25234,#25235,#25236,#25237,#25238,#25239,
#25240,#25241,#25242,#25243,#25244,#25245,#25246,#25247,#25248,#25249,#25250,
#25251,#25252,#25253,#25254,#25255,#25256,#25257),.UNSPECIFIED.,.F.,.F.)
B_SPLINE_CURVE_WITH_KNOTS((6,1,1,1,1,1,1,1,1,1,1,1,1,1,1,1,1,1,1,1,1,1,
1,1,1,1,1,1,1,1,1,1,1,1,1,1,1,1,1,1,1,1,1,1,1,1,1,1,1,1,1,1,1,1,1,1,1,1,
1,1,1,1,1,1,1,6),(0.,0.0153846153846154,0.0307692307692308,0.0461538461538462,
0.0615384615384615,0.0769230769230769,0.0923076923076923,0.107692307692308,
0.123076923076923,0.138461538461538,0.153846153846154,0.169230769230769,
0.184615384615385,0.2,0.215384615384615,0.230769230769231,0.246153846153846,
0.261538461538462,0.276923076923077,0.292307692307692,0.307692307692308,
0.323076923076923,0.338461538461538,0.353846153846154,0.369230769230769,
0.384615384615385,0.4,0.415384615384615,0.430769230769231,0.446153846153846,
0.461538461538462,0.476923076923077,0.492307692307692,0.507692307692308,
0.523076923076923,0.538461538461538,0.553846153846154,0.569230769230769,
0.584615384615384,0.6,0.615384615384615,0.63076923076923,0.646153846153846,
0.661538461538461,0.676923076923076,0.692307692307692,0.707692307692307,
0.723076923076922,0.738461538461538,0.753846153846153,0.769230769230768,
0.784615384615384,0.799999999999999,0.815384615384614,0.83076923076923,
0.846153846153845,0.86153846153846,0.876923076923076,0.892307692307691,
0.907692307692306,0.923076923076922,0.938461538461537,0.953846153846152,
0.969230769230768,0.984615384615383,1.),.UNSPECIFIED.)
CURVE()
GEOMETRIC_REPRESENTATION_ITEM()
RATIONAL_B_SPLINE_CURVE((1.,1.,1.,1.,1.,1.,1.,1.,1.,1.,1.,1.,1.,1.,1.,1.,
1.,1.,1.,1.,1.,1.,1.,1.,1.,1.,1.,1.,1.,1.,1.,1.,1.,1.,1.,1.,1.,1.,1.,1.,
1.,1.,1.,1.,1.,1.,1.,1.,1.,1.,1.,1.,1.,1.,1.,1.,1.,1.,1.,1.,1.,1.,1.,1.,
1.,1.,1.,1.,1.,1.))
REPRESENTATION_ITEM('')
);
#84=(
BOUNDED_CURVE()
B_SPLINE_CURVE(5,(#25261,#25262,#25263,#25264,#25265,#25266,#25267,#25268,
#25269,#25270,#25271,#25272,#25273,#25274,#25275,#25276,#25277,#25278,#25279,
#25280,#25281,#25282,#25283,#25284,#25285,#25286,#25287,#25288,#25289,#25290,
#25291,#25292,#25293,#25294,#25295,#25296,#25297,#25298,#25299,#25300,#25301,
#25302,#25303,#25304,#25305,#25306,#25307,#25308,#25309,#25310,#25311,#25312,
#25313,#25314,#25315,#25316,#25317,#25318,#25319,#25320,#25321,#25322,#25323,
#25324,#25325,#25326,#25327,#25328,#25329,#25330),.UNSPECIFIED.,.F.,.F.)
B_SPLINE_CURVE_WITH_KNOTS((6,1,1,1,1,1,1,1,1,1,1,1,1,1,1,1,1,1,1,1,1,1,
1,1,1,1,1,1,1,1,1,1,1,1,1,1,1,1,1,1,1,1,1,1,1,1,1,1,1,1,1,1,1,1,1,1,1,1,
1,1,1,1,1,1,1,6),(0.,0.0153846153846154,0.0307692307692308,0.0461538461538462,
0.0615384615384615,0.0769230769230769,0.0923076923076923,0.107692307692308,
0.123076923076923,0.138461538461538,0.153846153846154,0.169230769230769,
0.184615384615385,0.2,0.215384615384615,0.230769230769231,0.246153846153846,
0.261538461538462,0.276923076923077,0.292307692307692,0.307692307692308,
0.323076923076923,0.338461538461538,0.353846153846154,0.369230769230769,
0.384615384615385,0.4,0.415384615384615,0.430769230769231,0.446153846153846,
0.461538461538462,0.476923076923077,0.492307692307692,0.507692307692308,
0.523076923076923,0.538461538461538,0.553846153846154,0.569230769230769,
0.584615384615384,0.6,0.615384615384615,0.63076923076923,0.646153846153846,
0.661538461538461,0.676923076923076,0.692307692307692,0.707692307692307,
0.723076923076922,0.738461538461538,0.753846153846153,0.769230769230768,
0.784615384615384,0.799999999999999,0.815384615384614,0.83076923076923,
0.846153846153845,0.86153846153846,0.876923076923076,0.892307692307691,
0.907692307692306,0.923076923076922,0.938461538461537,0.953846153846152,
0.969230769230768,0.984615384615383,1.),.UNSPECIFIED.)
CURVE()
GEOMETRIC_REPRESENTATION_ITEM()
RATIONAL_B_SPLINE_CURVE((1.,1.,1.,1.,1.,1.,1.,1.,1.,1.,1.,1.,1.,1.,1.,1.,
1.,1.,1.,1.,1.,1.,1.,1.,1.,1.,1.,1.,1.,1.,1.,1.,1.,1.,1.,1.,1.,1.,1.,1.,
1.,1.,1.,1.,1.,1.,1.,1.,1.,1.,1.,1.,1.,1.,1.,1.,1.,1.,1.,1.,1.,1.,1.,1.,
1.,1.,1.,1.,1.,1.))
REPRESENTATION_ITEM('')
);
#85=(
BOUNDED_CURVE()
B_SPLINE_CURVE(5,(#25334,#25335,#25336,#25337,#25338,#25339,#25340,#25341,
#25342,#25343,#25344,#25345,#25346,#25347,#25348,#25349,#25350,#25351,#25352,
#25353,#25354,#25355,#25356,#25357,#25358,#25359,#25360,#25361,#25362,#25363,
#25364,#25365,#25366,#25367,#25368,#25369,#25370,#25371,#25372,#25373,#25374,
#25375,#25376,#25377,#25378,#25379,#25380,#25381,#25382,#25383,#25384,#25385,
#25386,#25387,#25388,#25389,#25390,#25391,#25392,#25393,#25394,#25395,#25396,
#25397,#25398,#25399,#25400,#25401,#25402,#25403),.UNSPECIFIED.,.F.,.F.)
B_SPLINE_CURVE_WITH_KNOTS((6,1,1,1,1,1,1,1,1,1,1,1,1,1,1,1,1,1,1,1,1,1,
1,1,1,1,1,1,1,1,1,1,1,1,1,1,1,1,1,1,1,1,1,1,1,1,1,1,1,1,1,1,1,1,1,1,1,1,
1,1,1,1,1,1,1,6),(0.,0.0153846153846154,0.0307692307692308,0.0461538461538462,
0.0615384615384615,0.0769230769230769,0.0923076923076923,0.107692307692308,
0.123076923076923,0.138461538461538,0.153846153846154,0.169230769230769,
0.184615384615385,0.2,0.215384615384615,0.230769230769231,0.246153846153846,
0.261538461538462,0.276923076923077,0.292307692307692,0.307692307692308,
0.323076923076923,0.338461538461538,0.353846153846154,0.369230769230769,
0.384615384615385,0.4,0.415384615384615,0.430769230769231,0.446153846153846,
0.461538461538462,0.476923076923077,0.492307692307692,0.507692307692308,
0.523076923076923,0.538461538461538,0.553846153846154,0.569230769230769,
0.584615384615384,0.6,0.615384615384615,0.63076923076923,0.646153846153846,
0.661538461538461,0.676923076923076,0.692307692307692,0.707692307692307,
0.723076923076922,0.738461538461538,0.753846153846153,0.769230769230768,
0.784615384615384,0.799999999999999,0.815384615384614,0.83076923076923,
0.846153846153845,0.86153846153846,0.876923076923076,0.892307692307691,
0.907692307692306,0.923076923076922,0.938461538461537,0.953846153846152,
0.969230769230768,0.984615384615383,1.),.UNSPECIFIED.)
CURVE()
GEOMETRIC_REPRESENTATION_ITEM()
RATIONAL_B_SPLINE_CURVE((1.,1.,1.,1.,1.,1.,1.,1.,1.,1.,1.,1.,1.,1.,1.,1.,
1.,1.,1.,1.,1.,1.,1.,1.,1.,1.,1.,1.,1.,1.,1.,1.,1.,1.,1.,1.,1.,1.,1.,1.,
1.,1.,1.,1.,1.,1.,1.,1.,1.,1.,1.,1.,1.,1.,1.,1.,1.,1.,1.,1.,1.,1.,1.,1.,
1.,1.,1.,1.,1.,1.))
REPRESENTATION_ITEM('')
);
#86=(
BOUNDED_CURVE()
B_SPLINE_CURVE(5,(#25407,#25408,#25409,#25410,#25411,#25412,#25413,#25414,
#25415,#25416,#25417,#25418,#25419,#25420,#25421,#25422,#25423,#25424,#25425,
#25426,#25427,#25428,#25429,#25430,#25431,#25432,#25433,#25434,#25435,#25436,
#25437,#25438,#25439,#25440,#25441,#25442,#25443,#25444,#25445,#25446,#25447,
#25448,#25449,#25450,#25451,#25452,#25453,#25454,#25455,#25456,#25457,#25458,
#25459,#25460,#25461,#25462,#25463,#25464,#25465,#25466,#25467,#25468,#25469,
#25470,#25471,#25472,#25473,#25474,#25475,#25476),.UNSPECIFIED.,.F.,.F.)
B_SPLINE_CURVE_WITH_KNOTS((6,1,1,1,1,1,1,1,1,1,1,1,1,1,1,1,1,1,1,1,1,1,
1,1,1,1,1,1,1,1,1,1,1,1,1,1,1,1,1,1,1,1,1,1,1,1,1,1,1,1,1,1,1,1,1,1,1,1,
1,1,1,1,1,1,1,6),(0.,0.0153846153846154,0.0307692307692308,0.0461538461538462,
0.0615384615384615,0.0769230769230769,0.0923076923076923,0.107692307692308,
0.123076923076923,0.138461538461538,0.153846153846154,0.169230769230769,
0.184615384615385,0.2,0.215384615384615,0.230769230769231,0.246153846153846,
0.261538461538462,0.276923076923077,0.292307692307692,0.307692307692308,
0.323076923076923,0.338461538461538,0.353846153846154,0.369230769230769,
0.384615384615385,0.4,0.415384615384615,0.430769230769231,0.446153846153846,
0.461538461538462,0.476923076923077,0.492307692307692,0.507692307692308,
0.523076923076923,0.538461538461538,0.553846153846154,0.569230769230769,
0.584615384615384,0.6,0.615384615384615,0.63076923076923,0.646153846153846,
0.661538461538461,0.676923076923076,0.692307692307692,0.707692307692307,
0.723076923076922,0.738461538461538,0.753846153846153,0.769230769230768,
0.784615384615384,0.799999999999999,0.815384615384614,0.83076923076923,
0.846153846153845,0.86153846153846,0.876923076923076,0.892307692307691,
0.907692307692306,0.923076923076922,0.938461538461537,0.953846153846152,
0.969230769230768,0.984615384615383,1.),.UNSPECIFIED.)
CURVE()
GEOMETRIC_REPRESENTATION_ITEM()
RATIONAL_B_SPLINE_CURVE((1.,1.,1.,1.,1.,1.,1.,1.,1.,1.,1.,1.,1.,1.,1.,1.,
1.,1.,1.,1.,1.,1.,1.,1.,1.,1.,1.,1.,1.,1.,1.,1.,1.,1.,1.,1.,1.,1.,1.,1.,
1.,1.,1.,1.,1.,1.,1.,1.,1.,1.,1.,1.,1.,1.,1.,1.,1.,1.,1.,1.,1.,1.,1.,1.,
1.,1.,1.,1.,1.,1.))
REPRESENTATION_ITEM('')
);
#87=(
BOUNDED_CURVE()
B_SPLINE_CURVE(5,(#25480,#25481,#25482,#25483,#25484,#25485,#25486,#25487,
#25488,#25489,#25490,#25491,#25492,#25493,#25494,#25495,#25496,#25497,#25498,
#25499,#25500,#25501,#25502,#25503,#25504,#25505,#25506,#25507,#25508,#25509,
#25510,#25511,#25512,#25513,#25514,#25515,#25516,#25517,#25518,#25519,#25520,
#25521,#25522,#25523,#25524,#25525,#25526,#25527,#25528,#25529,#25530,#25531,
#25532,#25533,#25534,#25535,#25536,#25537,#25538,#25539,#25540,#25541,#25542,
#25543,#25544,#25545,#25546,#25547,#25548,#25549),.UNSPECIFIED.,.F.,.F.)
B_SPLINE_CURVE_WITH_KNOTS((6,1,1,1,1,1,1,1,1,1,1,1,1,1,1,1,1,1,1,1,1,1,
1,1,1,1,1,1,1,1,1,1,1,1,1,1,1,1,1,1,1,1,1,1,1,1,1,1,1,1,1,1,1,1,1,1,1,1,
1,1,1,1,1,1,1,6),(0.,0.0153846153846154,0.0307692307692308,0.0461538461538462,
0.0615384615384615,0.0769230769230769,0.0923076923076923,0.107692307692308,
0.123076923076923,0.138461538461538,0.153846153846154,0.169230769230769,
0.184615384615385,0.2,0.215384615384615,0.230769230769231,0.246153846153846,
0.261538461538462,0.276923076923077,0.292307692307692,0.307692307692308,
0.323076923076923,0.338461538461538,0.353846153846154,0.369230769230769,
0.384615384615385,0.4,0.415384615384615,0.430769230769231,0.446153846153846,
0.461538461538462,0.476923076923077,0.492307692307692,0.507692307692308,
0.523076923076923,0.538461538461538,0.553846153846154,0.569230769230769,
0.584615384615384,0.6,0.615384615384615,0.63076923076923,0.646153846153846,
0.661538461538461,0.676923076923076,0.692307692307692,0.707692307692307,
0.723076923076922,0.738461538461538,0.753846153846153,0.769230769230768,
0.784615384615384,0.799999999999999,0.815384615384614,0.83076923076923,
0.846153846153845,0.86153846153846,0.876923076923076,0.892307692307691,
0.907692307692306,0.923076923076922,0.938461538461537,0.953846153846152,
0.969230769230768,0.984615384615383,1.),.UNSPECIFIED.)
CURVE()
GEOMETRIC_REPRESENTATION_ITEM()
RATIONAL_B_SPLINE_CURVE((1.,1.,1.,1.,1.,1.,1.,1.,1.,1.,1.,1.,1.,1.,1.,1.,
1.,1.,1.,1.,1.,1.,1.,1.,1.,1.,1.,1.,1.,1.,1.,1.,1.,1.,1.,1.,1.,1.,1.,1.,
1.,1.,1.,1.,1.,1.,1.,1.,1.,1.,1.,1.,1.,1.,1.,1.,1.,1.,1.,1.,1.,1.,1.,1.,
1.,1.,1.,1.,1.,1.))
REPRESENTATION_ITEM('')
);
#88=(
BOUNDED_CURVE()
B_SPLINE_CURVE(5,(#25553,#25554,#25555,#25556,#25557,#25558,#25559,#25560,
#25561,#25562,#25563,#25564,#25565,#25566,#25567,#25568,#25569,#25570,#25571,
#25572,#25573,#25574,#25575,#25576,#25577,#25578,#25579,#25580,#25581,#25582,
#25583,#25584,#25585,#25586,#25587,#25588,#25589,#25590,#25591,#25592,#25593,
#25594,#25595,#25596,#25597,#25598,#25599,#25600,#25601,#25602,#25603,#25604,
#25605,#25606,#25607,#25608,#25609,#25610,#25611,#25612,#25613,#25614,#25615,
#25616,#25617,#25618,#25619,#25620,#25621,#25622),.UNSPECIFIED.,.F.,.F.)
B_SPLINE_CURVE_WITH_KNOTS((6,1,1,1,1,1,1,1,1,1,1,1,1,1,1,1,1,1,1,1,1,1,
1,1,1,1,1,1,1,1,1,1,1,1,1,1,1,1,1,1,1,1,1,1,1,1,1,1,1,1,1,1,1,1,1,1,1,1,
1,1,1,1,1,1,1,6),(0.,0.0153846153846154,0.0307692307692308,0.0461538461538462,
0.0615384615384615,0.0769230769230769,0.0923076923076923,0.107692307692308,
0.123076923076923,0.138461538461538,0.153846153846154,0.169230769230769,
0.184615384615385,0.2,0.215384615384615,0.230769230769231,0.246153846153846,
0.261538461538462,0.276923076923077,0.292307692307692,0.307692307692308,
0.323076923076923,0.338461538461538,0.353846153846154,0.369230769230769,
0.384615384615385,0.4,0.415384615384615,0.430769230769231,0.446153846153846,
0.461538461538462,0.476923076923077,0.492307692307692,0.507692307692308,
0.523076923076923,0.538461538461538,0.553846153846154,0.569230769230769,
0.584615384615384,0.6,0.615384615384615,0.63076923076923,0.646153846153846,
0.661538461538461,0.676923076923076,0.692307692307692,0.707692307692307,
0.723076923076922,0.738461538461538,0.753846153846153,0.769230769230768,
0.784615384615384,0.799999999999999,0.815384615384614,0.83076923076923,
0.846153846153845,0.86153846153846,0.876923076923076,0.892307692307691,
0.907692307692306,0.923076923076922,0.938461538461537,0.953846153846152,
0.969230769230768,0.984615384615383,1.),.UNSPECIFIED.)
CURVE()
GEOMETRIC_REPRESENTATION_ITEM()
RATIONAL_B_SPLINE_CURVE((1.,1.,1.,1.,1.,1.,1.,1.,1.,1.,1.,1.,1.,1.,1.,1.,
1.,1.,1.,1.,1.,1.,1.,1.,1.,1.,1.,1.,1.,1.,1.,1.,1.,1.,1.,1.,1.,1.,1.,1.,
1.,1.,1.,1.,1.,1.,1.,1.,1.,1.,1.,1.,1.,1.,1.,1.,1.,1.,1.,1.,1.,1.,1.,1.,
1.,1.,1.,1.,1.,1.))
REPRESENTATION_ITEM('')
);
#89=(
BOUNDED_CURVE()
B_SPLINE_CURVE(5,(#25626,#25627,#25628,#25629,#25630,#25631,#25632,#25633,
#25634,#25635,#25636,#25637,#25638,#25639,#25640,#25641,#25642,#25643,#25644,
#25645,#25646,#25647,#25648,#25649,#25650,#25651,#25652,#25653,#25654,#25655,
#25656,#25657,#25658,#25659,#25660,#25661,#25662,#25663,#25664,#25665,#25666,
#25667,#25668,#25669,#25670,#25671,#25672,#25673,#25674,#25675,#25676,#25677,
#25678,#25679,#25680,#25681,#25682,#25683,#25684,#25685,#25686,#25687,#25688,
#25689,#25690,#25691,#25692,#25693,#25694,#25695),.UNSPECIFIED.,.F.,.F.)
B_SPLINE_CURVE_WITH_KNOTS((6,1,1,1,1,1,1,1,1,1,1,1,1,1,1,1,1,1,1,1,1,1,
1,1,1,1,1,1,1,1,1,1,1,1,1,1,1,1,1,1,1,1,1,1,1,1,1,1,1,1,1,1,1,1,1,1,1,1,
1,1,1,1,1,1,1,6),(0.,0.0153846153846154,0.0307692307692308,0.0461538461538462,
0.0615384615384615,0.0769230769230769,0.0923076923076923,0.107692307692308,
0.123076923076923,0.138461538461538,0.153846153846154,0.169230769230769,
0.184615384615385,0.2,0.215384615384615,0.230769230769231,0.246153846153846,
0.261538461538462,0.276923076923077,0.292307692307692,0.307692307692308,
0.323076923076923,0.338461538461538,0.353846153846154,0.369230769230769,
0.384615384615385,0.4,0.415384615384615,0.430769230769231,0.446153846153846,
0.461538461538462,0.476923076923077,0.492307692307692,0.507692307692308,
0.523076923076923,0.538461538461538,0.553846153846154,0.569230769230769,
0.584615384615384,0.6,0.615384615384615,0.63076923076923,0.646153846153846,
0.661538461538461,0.676923076923076,0.692307692307692,0.707692307692307,
0.723076923076922,0.738461538461538,0.753846153846153,0.769230769230768,
0.784615384615384,0.799999999999999,0.815384615384614,0.83076923076923,
0.846153846153845,0.86153846153846,0.876923076923076,0.892307692307691,
0.907692307692306,0.923076923076922,0.938461538461537,0.953846153846152,
0.969230769230768,0.984615384615383,1.),.UNSPECIFIED.)
CURVE()
GEOMETRIC_REPRESENTATION_ITEM()
RATIONAL_B_SPLINE_CURVE((1.,1.,1.,1.,1.,1.,1.,1.,1.,1.,1.,1.,1.,1.,1.,1.,
1.,1.,1.,1.,1.,1.,1.,1.,1.,1.,1.,1.,1.,1.,1.,1.,1.,1.,1.,1.,1.,1.,1.,1.,
1.,1.,1.,1.,1.,1.,1.,1.,1.,1.,1.,1.,1.,1.,1.,1.,1.,1.,1.,1.,1.,1.,1.,1.,
1.,1.,1.,1.,1.,1.))
REPRESENTATION_ITEM('')
);
#90=(
BOUNDED_CURVE()
B_SPLINE_CURVE(5,(#25698,#25699,#25700,#25701,#25702,#25703,#25704,#25705,
#25706,#25707,#25708,#25709,#25710,#25711,#25712,#25713,#25714,#25715,#25716,
#25717,#25718,#25719,#25720,#25721,#25722,#25723,#25724,#25725,#25726,#25727,
#25728,#25729,#25730,#25731,#25732,#25733,#25734,#25735,#25736,#25737,#25738,
#25739,#25740,#25741,#25742,#25743,#25744,#25745,#25746,#25747,#25748,#25749,
#25750,#25751,#25752,#25753,#25754,#25755,#25756,#25757,#25758,#25759,#25760,
#25761,#25762,#25763,#25764,#25765,#25766,#25767),.UNSPECIFIED.,.F.,.F.)
B_SPLINE_CURVE_WITH_KNOTS((6,1,1,1,1,1,1,1,1,1,1,1,1,1,1,1,1,1,1,1,1,1,
1,1,1,1,1,1,1,1,1,1,1,1,1,1,1,1,1,1,1,1,1,1,1,1,1,1,1,1,1,1,1,1,1,1,1,1,
1,1,1,1,1,1,1,6),(0.,0.0153846153846154,0.0307692307692308,0.0461538461538462,
0.0615384615384615,0.0769230769230769,0.0923076923076923,0.107692307692308,
0.123076923076923,0.138461538461538,0.153846153846154,0.169230769230769,
0.184615384615385,0.2,0.215384615384615,0.230769230769231,0.246153846153846,
0.261538461538462,0.276923076923077,0.292307692307692,0.307692307692308,
0.323076923076923,0.338461538461538,0.353846153846154,0.369230769230769,
0.384615384615385,0.4,0.415384615384615,0.430769230769231,0.446153846153846,
0.461538461538462,0.476923076923077,0.492307692307692,0.507692307692308,
0.523076923076923,0.538461538461538,0.553846153846154,0.569230769230769,
0.584615384615384,0.6,0.615384615384615,0.63076923076923,0.646153846153846,
0.661538461538461,0.676923076923076,0.692307692307692,0.707692307692307,
0.723076923076922,0.738461538461538,0.753846153846153,0.769230769230768,
0.784615384615384,0.799999999999999,0.815384615384614,0.83076923076923,
0.846153846153845,0.86153846153846,0.876923076923076,0.892307692307691,
0.907692307692306,0.923076923076922,0.938461538461537,0.953846153846152,
0.969230769230768,0.984615384615383,1.),.UNSPECIFIED.)
CURVE()
GEOMETRIC_REPRESENTATION_ITEM()
RATIONAL_B_SPLINE_CURVE((1.,1.,1.,1.,1.,1.,1.,1.,1.,1.,1.,1.,1.,1.,1.,1.,
1.,1.,1.,1.,1.,1.,1.,1.,1.,1.,1.,1.,1.,1.,1.,1.,1.,1.,1.,1.,1.,1.,1.,1.,
1.,1.,1.,1.,1.,1.,1.,1.,1.,1.,1.,1.,1.,1.,1.,1.,1.,1.,1.,1.,1.,1.,1.,1.,
1.,1.,1.,1.,1.,1.))
REPRESENTATION_ITEM('')
);
#91=(
BOUNDED_CURVE()
B_SPLINE_CURVE(5,(#25921,#25922,#25923,#25924,#25925,#25926,#25927,#25928,
#25929,#25930,#25931,#25932,#25933,#25934,#25935,#25936,#25937,#25938,#25939,
#25940,#25941,#25942,#25943,#25944,#25945,#25946,#25947,#25948,#25949,#25950,
#25951,#25952,#25953,#25954,#25955,#25956,#25957,#25958,#25959,#25960,#25961,
#25962,#25963,#25964,#25965,#25966,#25967,#25968,#25969,#25970,#25971,#25972,
#25973,#25974,#25975,#25976,#25977,#25978,#25979,#25980,#25981,#25982,#25983,
#25984,#25985,#25986,#25987,#25988,#25989,#25990),.UNSPECIFIED.,.F.,.F.)
B_SPLINE_CURVE_WITH_KNOTS((6,1,1,1,1,1,1,1,1,1,1,1,1,1,1,1,1,1,1,1,1,1,
1,1,1,1,1,1,1,1,1,1,1,1,1,1,1,1,1,1,1,1,1,1,1,1,1,1,1,1,1,1,1,1,1,1,1,1,
1,1,1,1,1,1,1,6),(-1.,-0.984615384615383,-0.969230769230768,-0.953846153846152,
-0.938461538461537,-0.923076923076922,-0.907692307692306,-0.892307692307691,
-0.876923076923076,-0.86153846153846,-0.846153846153845,-0.83076923076923,
-0.815384615384614,-0.799999999999999,-0.784615384615384,-0.769230769230768,
-0.753846153846153,-0.738461538461538,-0.723076923076922,-0.707692307692307,
-0.692307692307692,-0.676923076923076,-0.661538461538461,-0.646153846153846,
-0.63076923076923,-0.615384615384615,-0.6,-0.584615384615384,-0.569230769230769,
-0.553846153846154,-0.538461538461538,-0.523076923076923,-0.507692307692308,
-0.492307692307692,-0.476923076923077,-0.461538461538462,-0.446153846153846,
-0.430769230769231,-0.415384615384615,-0.4,-0.384615384615385,-0.369230769230769,
-0.353846153846154,-0.338461538461538,-0.323076923076923,-0.307692307692308,
-0.292307692307692,-0.276923076923077,-0.261538461538462,-0.246153846153846,
-0.230769230769231,-0.215384615384615,-0.2,-0.184615384615385,-0.169230769230769,
-0.153846153846154,-0.138461538461538,-0.123076923076923,-0.107692307692308,
-0.0923076923076923,-0.0769230769230769,-0.0615384615384615,-0.0461538461538462,
-0.0307692307692308,-0.0153846153846154,0.),.UNSPECIFIED.)
CURVE()
GEOMETRIC_REPRESENTATION_ITEM()
RATIONAL_B_SPLINE_CURVE((1.,1.,1.,1.,1.,1.,1.,1.,1.,1.,1.,1.,1.,1.,1.,1.,
1.,1.,1.,1.,1.,1.,1.,1.,1.,1.,1.,1.,1.,1.,1.,1.,1.,1.,1.,1.,1.,1.,1.,1.,
1.,1.,1.,1.,1.,1.,1.,1.,1.,1.,1.,1.,1.,1.,1.,1.,1.,1.,1.,1.,1.,1.,1.,1.,
1.,1.,1.,1.,1.,1.))
REPRESENTATION_ITEM('')
);
#92=(
BOUNDED_CURVE()
B_SPLINE_CURVE(5,(#26137,#26138,#26139,#26140,#26141,#26142,#26143,#26144,
#26145,#26146,#26147,#26148,#26149,#26150,#26151,#26152,#26153,#26154,#26155,
#26156,#26157,#26158,#26159,#26160,#26161,#26162,#26163,#26164,#26165,#26166,
#26167,#26168,#26169,#26170,#26171,#26172,#26173,#26174,#26175,#26176,#26177,
#26178,#26179,#26180,#26181,#26182,#26183,#26184,#26185,#26186,#26187,#26188,
#26189,#26190,#26191,#26192,#26193,#26194,#26195,#26196,#26197,#26198,#26199,
#26200,#26201,#26202,#26203,#26204,#26205,#26206),.UNSPECIFIED.,.F.,.F.)
B_SPLINE_CURVE_WITH_KNOTS((6,1,1,1,1,1,1,1,1,1,1,1,1,1,1,1,1,1,1,1,1,1,
1,1,1,1,1,1,1,1,1,1,1,1,1,1,1,1,1,1,1,1,1,1,1,1,1,1,1,1,1,1,1,1,1,1,1,1,
1,1,1,1,1,1,1,6),(-1.,-0.984615384615383,-0.969230769230768,-0.953846153846152,
-0.938461538461537,-0.923076923076922,-0.907692307692306,-0.892307692307691,
-0.876923076923076,-0.86153846153846,-0.846153846153845,-0.83076923076923,
-0.815384615384614,-0.799999999999999,-0.784615384615384,-0.769230769230768,
-0.753846153846153,-0.738461538461538,-0.723076923076922,-0.707692307692307,
-0.692307692307692,-0.676923076923076,-0.661538461538461,-0.646153846153846,
-0.63076923076923,-0.615384615384615,-0.6,-0.584615384615384,-0.569230769230769,
-0.553846153846154,-0.538461538461538,-0.523076923076923,-0.507692307692308,
-0.492307692307692,-0.476923076923077,-0.461538461538462,-0.446153846153846,
-0.430769230769231,-0.415384615384615,-0.4,-0.384615384615385,-0.369230769230769,
-0.353846153846154,-0.338461538461538,-0.323076923076923,-0.307692307692308,
-0.292307692307692,-0.276923076923077,-0.261538461538462,-0.246153846153846,
-0.230769230769231,-0.215384615384615,-0.2,-0.184615384615385,-0.169230769230769,
-0.153846153846154,-0.138461538461538,-0.123076923076923,-0.107692307692308,
-0.0923076923076923,-0.0769230769230769,-0.0615384615384615,-0.0461538461538462,
-0.0307692307692308,-0.0153846153846154,0.),.UNSPECIFIED.)
CURVE()
GEOMETRIC_REPRESENTATION_ITEM()
RATIONAL_B_SPLINE_CURVE((1.,1.,1.,1.,1.,1.,1.,1.,1.,1.,1.,1.,1.,1.,1.,1.,
1.,1.,1.,1.,1.,1.,1.,1.,1.,1.,1.,1.,1.,1.,1.,1.,1.,1.,1.,1.,1.,1.,1.,1.,
1.,1.,1.,1.,1.,1.,1.,1.,1.,1.,1.,1.,1.,1.,1.,1.,1.,1.,1.,1.,1.,1.,1.,1.,
1.,1.,1.,1.,1.,1.))
REPRESENTATION_ITEM('')
);
#93=(
BOUNDED_CURVE()
B_SPLINE_CURVE(5,(#26353,#26354,#26355,#26356,#26357,#26358,#26359,#26360,
#26361,#26362,#26363,#26364,#26365,#26366,#26367,#26368,#26369,#26370,#26371,
#26372,#26373,#26374,#26375,#26376,#26377,#26378,#26379,#26380,#26381,#26382,
#26383,#26384,#26385,#26386,#26387,#26388,#26389,#26390,#26391,#26392,#26393,
#26394,#26395,#26396,#26397,#26398,#26399,#26400,#26401,#26402,#26403,#26404,
#26405,#26406,#26407,#26408,#26409,#26410,#26411,#26412,#26413,#26414,#26415,
#26416,#26417,#26418,#26419,#26420,#26421,#26422),.UNSPECIFIED.,.F.,.F.)
B_SPLINE_CURVE_WITH_KNOTS((6,1,1,1,1,1,1,1,1,1,1,1,1,1,1,1,1,1,1,1,1,1,
1,1,1,1,1,1,1,1,1,1,1,1,1,1,1,1,1,1,1,1,1,1,1,1,1,1,1,1,1,1,1,1,1,1,1,1,
1,1,1,1,1,1,1,6),(-1.,-0.984615384615383,-0.969230769230768,-0.953846153846152,
-0.938461538461537,-0.923076923076922,-0.907692307692306,-0.892307692307691,
-0.876923076923076,-0.86153846153846,-0.846153846153845,-0.83076923076923,
-0.815384615384614,-0.799999999999999,-0.784615384615384,-0.769230769230768,
-0.753846153846153,-0.738461538461538,-0.723076923076922,-0.707692307692307,
-0.692307692307692,-0.676923076923076,-0.661538461538461,-0.646153846153846,
-0.63076923076923,-0.615384615384615,-0.6,-0.584615384615384,-0.569230769230769,
-0.553846153846154,-0.538461538461538,-0.523076923076923,-0.507692307692308,
-0.492307692307692,-0.476923076923077,-0.461538461538462,-0.446153846153846,
-0.430769230769231,-0.415384615384615,-0.4,-0.384615384615385,-0.369230769230769,
-0.353846153846154,-0.338461538461538,-0.323076923076923,-0.307692307692308,
-0.292307692307692,-0.276923076923077,-0.261538461538462,-0.246153846153846,
-0.230769230769231,-0.215384615384615,-0.2,-0.184615384615385,-0.169230769230769,
-0.153846153846154,-0.138461538461538,-0.123076923076923,-0.107692307692308,
-0.0923076923076923,-0.0769230769230769,-0.0615384615384615,-0.0461538461538462,
-0.0307692307692308,-0.0153846153846154,0.),.UNSPECIFIED.)
CURVE()
GEOMETRIC_REPRESENTATION_ITEM()
RATIONAL_B_SPLINE_CURVE((1.,1.,1.,1.,1.,1.,1.,1.,1.,1.,1.,1.,1.,1.,1.,1.,
1.,1.,1.,1.,1.,1.,1.,1.,1.,1.,1.,1.,1.,1.,1.,1.,1.,1.,1.,1.,1.,1.,1.,1.,
1.,1.,1.,1.,1.,1.,1.,1.,1.,1.,1.,1.,1.,1.,1.,1.,1.,1.,1.,1.,1.,1.,1.,1.,
1.,1.,1.,1.,1.,1.))
REPRESENTATION_ITEM('')
);
#94=(
BOUNDED_CURVE()
B_SPLINE_CURVE(5,(#26569,#26570,#26571,#26572,#26573,#26574,#26575,#26576,
#26577,#26578,#26579,#26580,#26581,#26582,#26583,#26584,#26585,#26586,#26587,
#26588,#26589,#26590,#26591,#26592,#26593,#26594,#26595,#26596,#26597,#26598,
#26599,#26600,#26601,#26602,#26603,#26604,#26605,#26606,#26607,#26608,#26609,
#26610,#26611,#26612,#26613,#26614,#26615,#26616,#26617,#26618,#26619,#26620,
#26621,#26622,#26623,#26624,#26625,#26626,#26627,#26628,#26629,#26630,#26631,
#26632,#26633,#26634,#26635,#26636,#26637,#26638),.UNSPECIFIED.,.F.,.F.)
B_SPLINE_CURVE_WITH_KNOTS((6,1,1,1,1,1,1,1,1,1,1,1,1,1,1,1,1,1,1,1,1,1,
1,1,1,1,1,1,1,1,1,1,1,1,1,1,1,1,1,1,1,1,1,1,1,1,1,1,1,1,1,1,1,1,1,1,1,1,
1,1,1,1,1,1,1,6),(-1.,-0.984615384615383,-0.969230769230768,-0.953846153846152,
-0.938461538461537,-0.923076923076922,-0.907692307692306,-0.892307692307691,
-0.876923076923076,-0.86153846153846,-0.846153846153845,-0.83076923076923,
-0.815384615384614,-0.799999999999999,-0.784615384615384,-0.769230769230768,
-0.753846153846153,-0.738461538461538,-0.723076923076922,-0.707692307692307,
-0.692307692307692,-0.676923076923076,-0.661538461538461,-0.646153846153846,
-0.63076923076923,-0.615384615384615,-0.6,-0.584615384615384,-0.569230769230769,
-0.553846153846154,-0.538461538461538,-0.523076923076923,-0.507692307692308,
-0.492307692307692,-0.476923076923077,-0.461538461538462,-0.446153846153846,
-0.430769230769231,-0.415384615384615,-0.4,-0.384615384615385,-0.369230769230769,
-0.353846153846154,-0.338461538461538,-0.323076923076923,-0.307692307692308,
-0.292307692307692,-0.276923076923077,-0.261538461538462,-0.246153846153846,
-0.230769230769231,-0.215384615384615,-0.2,-0.184615384615385,-0.169230769230769,
-0.153846153846154,-0.138461538461538,-0.123076923076923,-0.107692307692308,
-0.0923076923076923,-0.0769230769230769,-0.0615384615384615,-0.0461538461538462,
-0.0307692307692308,-0.0153846153846154,0.),.UNSPECIFIED.)
CURVE()
GEOMETRIC_REPRESENTATION_ITEM()
RATIONAL_B_SPLINE_CURVE((1.,1.,1.,1.,1.,1.,1.,1.,1.,1.,1.,1.,1.,1.,1.,1.,
1.,1.,1.,1.,1.,1.,1.,1.,1.,1.,1.,1.,1.,1.,1.,1.,1.,1.,1.,1.,1.,1.,1.,1.,
1.,1.,1.,1.,1.,1.,1.,1.,1.,1.,1.,1.,1.,1.,1.,1.,1.,1.,1.,1.,1.,1.,1.,1.,
1.,1.,1.,1.,1.,1.))
REPRESENTATION_ITEM('')
);
#95=(
BOUNDED_CURVE()
B_SPLINE_CURVE(5,(#26785,#26786,#26787,#26788,#26789,#26790,#26791,#26792,
#26793,#26794,#26795,#26796,#26797,#26798,#26799,#26800,#26801,#26802,#26803,
#26804,#26805,#26806,#26807,#26808,#26809,#26810,#26811,#26812,#26813,#26814,
#26815,#26816,#26817,#26818,#26819,#26820,#26821,#26822,#26823,#26824,#26825,
#26826,#26827,#26828,#26829,#26830,#26831,#26832,#26833,#26834,#26835,#26836,
#26837,#26838,#26839,#26840,#26841,#26842,#26843,#26844,#26845,#26846,#26847,
#26848,#26849,#26850,#26851,#26852,#26853,#26854),.UNSPECIFIED.,.F.,.F.)
B_SPLINE_CURVE_WITH_KNOTS((6,1,1,1,1,1,1,1,1,1,1,1,1,1,1,1,1,1,1,1,1,1,
1,1,1,1,1,1,1,1,1,1,1,1,1,1,1,1,1,1,1,1,1,1,1,1,1,1,1,1,1,1,1,1,1,1,1,1,
1,1,1,1,1,1,1,6),(-1.,-0.984615384615383,-0.969230769230768,-0.953846153846152,
-0.938461538461537,-0.923076923076922,-0.907692307692306,-0.892307692307691,
-0.876923076923076,-0.86153846153846,-0.846153846153845,-0.83076923076923,
-0.815384615384614,-0.799999999999999,-0.784615384615384,-0.769230769230768,
-0.753846153846153,-0.738461538461538,-0.723076923076922,-0.707692307692307,
-0.692307692307692,-0.676923076923076,-0.661538461538461,-0.646153846153846,
-0.63076923076923,-0.615384615384615,-0.6,-0.584615384615384,-0.569230769230769,
-0.553846153846154,-0.538461538461538,-0.523076923076923,-0.507692307692308,
-0.492307692307692,-0.476923076923077,-0.461538461538462,-0.446153846153846,
-0.430769230769231,-0.415384615384615,-0.4,-0.384615384615385,-0.369230769230769,
-0.353846153846154,-0.338461538461538,-0.323076923076923,-0.307692307692308,
-0.292307692307692,-0.276923076923077,-0.261538461538462,-0.246153846153846,
-0.230769230769231,-0.215384615384615,-0.2,-0.184615384615385,-0.169230769230769,
-0.153846153846154,-0.138461538461538,-0.123076923076923,-0.107692307692308,
-0.0923076923076923,-0.0769230769230769,-0.0615384615384615,-0.0461538461538462,
-0.0307692307692308,-0.0153846153846154,0.),.UNSPECIFIED.)
CURVE()
GEOMETRIC_REPRESENTATION_ITEM()
RATIONAL_B_SPLINE_CURVE((1.,1.,1.,1.,1.,1.,1.,1.,1.,1.,1.,1.,1.,1.,1.,1.,
1.,1.,1.,1.,1.,1.,1.,1.,1.,1.,1.,1.,1.,1.,1.,1.,1.,1.,1.,1.,1.,1.,1.,1.,
1.,1.,1.,1.,1.,1.,1.,1.,1.,1.,1.,1.,1.,1.,1.,1.,1.,1.,1.,1.,1.,1.,1.,1.,
1.,1.,1.,1.,1.,1.))
REPRESENTATION_ITEM('')
);
#96=(
BOUNDED_CURVE()
B_SPLINE_CURVE(5,(#27001,#27002,#27003,#27004,#27005,#27006,#27007,#27008,
#27009,#27010,#27011,#27012,#27013,#27014,#27015,#27016,#27017,#27018,#27019,
#27020,#27021,#27022,#27023,#27024,#27025,#27026,#27027,#27028,#27029,#27030,
#27031,#27032,#27033,#27034,#27035,#27036,#27037,#27038,#27039,#27040,#27041,
#27042,#27043,#27044,#27045,#27046,#27047,#27048,#27049,#27050,#27051,#27052,
#27053,#27054,#27055,#27056,#27057,#27058,#27059,#27060,#27061,#27062,#27063,
#27064,#27065,#27066,#27067,#27068,#27069,#27070),.UNSPECIFIED.,.F.,.F.)
B_SPLINE_CURVE_WITH_KNOTS((6,1,1,1,1,1,1,1,1,1,1,1,1,1,1,1,1,1,1,1,1,1,
1,1,1,1,1,1,1,1,1,1,1,1,1,1,1,1,1,1,1,1,1,1,1,1,1,1,1,1,1,1,1,1,1,1,1,1,
1,1,1,1,1,1,1,6),(-1.,-0.984615384615383,-0.969230769230768,-0.953846153846152,
-0.938461538461537,-0.923076923076922,-0.907692307692306,-0.892307692307691,
-0.876923076923076,-0.86153846153846,-0.846153846153845,-0.83076923076923,
-0.815384615384614,-0.799999999999999,-0.784615384615384,-0.769230769230768,
-0.753846153846153,-0.738461538461538,-0.723076923076922,-0.707692307692307,
-0.692307692307692,-0.676923076923076,-0.661538461538461,-0.646153846153846,
-0.63076923076923,-0.615384615384615,-0.6,-0.584615384615384,-0.569230769230769,
-0.553846153846154,-0.538461538461538,-0.523076923076923,-0.507692307692308,
-0.492307692307692,-0.476923076923077,-0.461538461538462,-0.446153846153846,
-0.430769230769231,-0.415384615384615,-0.4,-0.384615384615385,-0.369230769230769,
-0.353846153846154,-0.338461538461538,-0.323076923076923,-0.307692307692308,
-0.292307692307692,-0.276923076923077,-0.261538461538462,-0.246153846153846,
-0.230769230769231,-0.215384615384615,-0.2,-0.184615384615385,-0.169230769230769,
-0.153846153846154,-0.138461538461538,-0.123076923076923,-0.107692307692308,
-0.0923076923076923,-0.0769230769230769,-0.0615384615384615,-0.0461538461538462,
-0.0307692307692308,-0.0153846153846154,0.),.UNSPECIFIED.)
CURVE()
GEOMETRIC_REPRESENTATION_ITEM()
RATIONAL_B_SPLINE_CURVE((1.,1.,1.,1.,1.,1.,1.,1.,1.,1.,1.,1.,1.,1.,1.,1.,
1.,1.,1.,1.,1.,1.,1.,1.,1.,1.,1.,1.,1.,1.,1.,1.,1.,1.,1.,1.,1.,1.,1.,1.,
1.,1.,1.,1.,1.,1.,1.,1.,1.,1.,1.,1.,1.,1.,1.,1.,1.,1.,1.,1.,1.,1.,1.,1.,
1.,1.,1.,1.,1.,1.))
REPRESENTATION_ITEM('')
);
#97=(
BOUNDED_CURVE()
B_SPLINE_CURVE(5,(#27217,#27218,#27219,#27220,#27221,#27222,#27223,#27224,
#27225,#27226,#27227,#27228,#27229,#27230,#27231,#27232,#27233,#27234,#27235,
#27236,#27237,#27238,#27239,#27240,#27241,#27242,#27243,#27244,#27245,#27246,
#27247,#27248,#27249,#27250,#27251,#27252,#27253,#27254,#27255,#27256,#27257,
#27258,#27259,#27260,#27261,#27262,#27263,#27264,#27265,#27266,#27267,#27268,
#27269,#27270,#27271,#27272,#27273,#27274,#27275,#27276,#27277,#27278,#27279,
#27280,#27281,#27282,#27283,#27284,#27285,#27286),.UNSPECIFIED.,.F.,.F.)
B_SPLINE_CURVE_WITH_KNOTS((6,1,1,1,1,1,1,1,1,1,1,1,1,1,1,1,1,1,1,1,1,1,
1,1,1,1,1,1,1,1,1,1,1,1,1,1,1,1,1,1,1,1,1,1,1,1,1,1,1,1,1,1,1,1,1,1,1,1,
1,1,1,1,1,1,1,6),(-1.,-0.984615384615383,-0.969230769230768,-0.953846153846152,
-0.938461538461537,-0.923076923076922,-0.907692307692306,-0.892307692307691,
-0.876923076923076,-0.86153846153846,-0.846153846153845,-0.83076923076923,
-0.815384615384614,-0.799999999999999,-0.784615384615384,-0.769230769230768,
-0.753846153846153,-0.738461538461538,-0.723076923076922,-0.707692307692307,
-0.692307692307692,-0.676923076923076,-0.661538461538461,-0.646153846153846,
-0.63076923076923,-0.615384615384615,-0.6,-0.584615384615384,-0.569230769230769,
-0.553846153846154,-0.538461538461538,-0.523076923076923,-0.507692307692308,
-0.492307692307692,-0.476923076923077,-0.461538461538462,-0.446153846153846,
-0.430769230769231,-0.415384615384615,-0.4,-0.384615384615385,-0.369230769230769,
-0.353846153846154,-0.338461538461538,-0.323076923076923,-0.307692307692308,
-0.292307692307692,-0.276923076923077,-0.261538461538462,-0.246153846153846,
-0.230769230769231,-0.215384615384615,-0.2,-0.184615384615385,-0.169230769230769,
-0.153846153846154,-0.138461538461538,-0.123076923076923,-0.107692307692308,
-0.0923076923076923,-0.0769230769230769,-0.0615384615384615,-0.0461538461538462,
-0.0307692307692308,-0.0153846153846154,0.),.UNSPECIFIED.)
CURVE()
GEOMETRIC_REPRESENTATION_ITEM()
RATIONAL_B_SPLINE_CURVE((1.,1.,1.,1.,1.,1.,1.,1.,1.,1.,1.,1.,1.,1.,1.,1.,
1.,1.,1.,1.,1.,1.,1.,1.,1.,1.,1.,1.,1.,1.,1.,1.,1.,1.,1.,1.,1.,1.,1.,1.,
1.,1.,1.,1.,1.,1.,1.,1.,1.,1.,1.,1.,1.,1.,1.,1.,1.,1.,1.,1.,1.,1.,1.,1.,
1.,1.,1.,1.,1.,1.))
REPRESENTATION_ITEM('')
);
#98=(
BOUNDED_CURVE()
B_SPLINE_CURVE(5,(#27433,#27434,#27435,#27436,#27437,#27438,#27439,#27440,
#27441,#27442,#27443,#27444,#27445,#27446,#27447,#27448,#27449,#27450,#27451,
#27452,#27453,#27454,#27455,#27456,#27457,#27458,#27459,#27460,#27461,#27462,
#27463,#27464,#27465,#27466,#27467,#27468,#27469,#27470,#27471,#27472,#27473,
#27474,#27475,#27476,#27477,#27478,#27479,#27480,#27481,#27482,#27483,#27484,
#27485,#27486,#27487,#27488,#27489,#27490,#27491,#27492,#27493,#27494,#27495,
#27496,#27497,#27498,#27499,#27500,#27501,#27502),.UNSPECIFIED.,.F.,.F.)
B_SPLINE_CURVE_WITH_KNOTS((6,1,1,1,1,1,1,1,1,1,1,1,1,1,1,1,1,1,1,1,1,1,
1,1,1,1,1,1,1,1,1,1,1,1,1,1,1,1,1,1,1,1,1,1,1,1,1,1,1,1,1,1,1,1,1,1,1,1,
1,1,1,1,1,1,1,6),(-1.,-0.984615384615383,-0.969230769230768,-0.953846153846152,
-0.938461538461537,-0.923076923076922,-0.907692307692306,-0.892307692307691,
-0.876923076923076,-0.86153846153846,-0.846153846153845,-0.83076923076923,
-0.815384615384614,-0.799999999999999,-0.784615384615384,-0.769230769230768,
-0.753846153846153,-0.738461538461538,-0.723076923076922,-0.707692307692307,
-0.692307692307692,-0.676923076923076,-0.661538461538461,-0.646153846153846,
-0.63076923076923,-0.615384615384615,-0.6,-0.584615384615384,-0.569230769230769,
-0.553846153846154,-0.538461538461538,-0.523076923076923,-0.507692307692308,
-0.492307692307692,-0.476923076923077,-0.461538461538462,-0.446153846153846,
-0.430769230769231,-0.415384615384615,-0.4,-0.384615384615385,-0.369230769230769,
-0.353846153846154,-0.338461538461538,-0.323076923076923,-0.307692307692308,
-0.292307692307692,-0.276923076923077,-0.261538461538462,-0.246153846153846,
-0.230769230769231,-0.215384615384615,-0.2,-0.184615384615385,-0.169230769230769,
-0.153846153846154,-0.138461538461538,-0.123076923076923,-0.107692307692308,
-0.0923076923076923,-0.0769230769230769,-0.0615384615384615,-0.0461538461538462,
-0.0307692307692308,-0.0153846153846154,0.),.UNSPECIFIED.)
CURVE()
GEOMETRIC_REPRESENTATION_ITEM()
RATIONAL_B_SPLINE_CURVE((1.,1.,1.,1.,1.,1.,1.,1.,1.,1.,1.,1.,1.,1.,1.,1.,
1.,1.,1.,1.,1.,1.,1.,1.,1.,1.,1.,1.,1.,1.,1.,1.,1.,1.,1.,1.,1.,1.,1.,1.,
1.,1.,1.,1.,1.,1.,1.,1.,1.,1.,1.,1.,1.,1.,1.,1.,1.,1.,1.,1.,1.,1.,1.,1.,
1.,1.,1.,1.,1.,1.))
REPRESENTATION_ITEM('')
);
#99=(
BOUNDED_CURVE()
B_SPLINE_CURVE(5,(#27649,#27650,#27651,#27652,#27653,#27654,#27655,#27656,
#27657,#27658,#27659,#27660,#27661,#27662,#27663,#27664,#27665,#27666,#27667,
#27668,#27669,#27670,#27671,#27672,#27673,#27674,#27675,#27676,#27677,#27678,
#27679,#27680,#27681,#27682,#27683,#27684,#27685,#27686,#27687,#27688,#27689,
#27690,#27691,#27692,#27693,#27694,#27695,#27696,#27697,#27698,#27699,#27700,
#27701,#27702,#27703,#27704,#27705,#27706,#27707,#27708,#27709,#27710,#27711,
#27712,#27713,#27714,#27715,#27716,#27717,#27718),.UNSPECIFIED.,.F.,.F.)
B_SPLINE_CURVE_WITH_KNOTS((6,1,1,1,1,1,1,1,1,1,1,1,1,1,1,1,1,1,1,1,1,1,
1,1,1,1,1,1,1,1,1,1,1,1,1,1,1,1,1,1,1,1,1,1,1,1,1,1,1,1,1,1,1,1,1,1,1,1,
1,1,1,1,1,1,1,6),(-1.,-0.984615384615383,-0.969230769230768,-0.953846153846152,
-0.938461538461537,-0.923076923076922,-0.907692307692306,-0.892307692307691,
-0.876923076923076,-0.86153846153846,-0.846153846153845,-0.83076923076923,
-0.815384615384614,-0.799999999999999,-0.784615384615384,-0.769230769230768,
-0.753846153846153,-0.738461538461538,-0.723076923076922,-0.707692307692307,
-0.692307692307692,-0.676923076923076,-0.661538461538461,-0.646153846153846,
-0.63076923076923,-0.615384615384615,-0.6,-0.584615384615384,-0.569230769230769,
-0.553846153846154,-0.538461538461538,-0.523076923076923,-0.507692307692308,
-0.492307692307692,-0.476923076923077,-0.461538461538462,-0.446153846153846,
-0.430769230769231,-0.415384615384615,-0.4,-0.384615384615385,-0.369230769230769,
-0.353846153846154,-0.338461538461538,-0.323076923076923,-0.307692307692308,
-0.292307692307692,-0.276923076923077,-0.261538461538462,-0.246153846153846,
-0.230769230769231,-0.215384615384615,-0.2,-0.184615384615385,-0.169230769230769,
-0.153846153846154,-0.138461538461538,-0.123076923076923,-0.107692307692308,
-0.0923076923076923,-0.0769230769230769,-0.0615384615384615,-0.0461538461538462,
-0.0307692307692308,-0.0153846153846154,0.),.UNSPECIFIED.)
CURVE()
GEOMETRIC_REPRESENTATION_ITEM()
RATIONAL_B_SPLINE_CURVE((1.,1.,1.,1.,1.,1.,1.,1.,1.,1.,1.,1.,1.,1.,1.,1.,
1.,1.,1.,1.,1.,1.,1.,1.,1.,1.,1.,1.,1.,1.,1.,1.,1.,1.,1.,1.,1.,1.,1.,1.,
1.,1.,1.,1.,1.,1.,1.,1.,1.,1.,1.,1.,1.,1.,1.,1.,1.,1.,1.,1.,1.,1.,1.,1.,
1.,1.,1.,1.,1.,1.))
REPRESENTATION_ITEM('')
);
#100=(
BOUNDED_CURVE()
B_SPLINE_CURVE(5,(#27865,#27866,#27867,#27868,#27869,#27870,#27871,#27872,
#27873,#27874,#27875,#27876,#27877,#27878,#27879,#27880,#27881,#27882,#27883,
#27884,#27885,#27886,#27887,#27888,#27889,#27890,#27891,#27892,#27893,#27894,
#27895,#27896,#27897,#27898,#27899,#27900,#27901,#27902,#27903,#27904,#27905,
#27906,#27907,#27908,#27909,#27910,#27911,#27912,#27913,#27914,#27915,#27916,
#27917,#27918,#27919,#27920,#27921,#27922,#27923,#27924,#27925,#27926,#27927,
#27928,#27929,#27930,#27931,#27932,#27933,#27934),.UNSPECIFIED.,.F.,.F.)
B_SPLINE_CURVE_WITH_KNOTS((6,1,1,1,1,1,1,1,1,1,1,1,1,1,1,1,1,1,1,1,1,1,
1,1,1,1,1,1,1,1,1,1,1,1,1,1,1,1,1,1,1,1,1,1,1,1,1,1,1,1,1,1,1,1,1,1,1,1,
1,1,1,1,1,1,1,6),(-1.,-0.984615384615383,-0.969230769230768,-0.953846153846152,
-0.938461538461537,-0.923076923076922,-0.907692307692306,-0.892307692307691,
-0.876923076923076,-0.86153846153846,-0.846153846153845,-0.83076923076923,
-0.815384615384614,-0.799999999999999,-0.784615384615384,-0.769230769230768,
-0.753846153846153,-0.738461538461538,-0.723076923076922,-0.707692307692307,
-0.692307692307692,-0.676923076923076,-0.661538461538461,-0.646153846153846,
-0.63076923076923,-0.615384615384615,-0.6,-0.584615384615384,-0.569230769230769,
-0.553846153846154,-0.538461538461538,-0.523076923076923,-0.507692307692308,
-0.492307692307692,-0.476923076923077,-0.461538461538462,-0.446153846153846,
-0.430769230769231,-0.415384615384615,-0.4,-0.384615384615385,-0.369230769230769,
-0.353846153846154,-0.338461538461538,-0.323076923076923,-0.307692307692308,
-0.292307692307692,-0.276923076923077,-0.261538461538462,-0.246153846153846,
-0.230769230769231,-0.215384615384615,-0.2,-0.184615384615385,-0.169230769230769,
-0.153846153846154,-0.138461538461538,-0.123076923076923,-0.107692307692308,
-0.0923076923076923,-0.0769230769230769,-0.0615384615384615,-0.0461538461538462,
-0.0307692307692308,-0.0153846153846154,0.),.UNSPECIFIED.)
CURVE()
GEOMETRIC_REPRESENTATION_ITEM()
RATIONAL_B_SPLINE_CURVE((1.,1.,1.,1.,1.,1.,1.,1.,1.,1.,1.,1.,1.,1.,1.,1.,
1.,1.,1.,1.,1.,1.,1.,1.,1.,1.,1.,1.,1.,1.,1.,1.,1.,1.,1.,1.,1.,1.,1.,1.,
1.,1.,1.,1.,1.,1.,1.,1.,1.,1.,1.,1.,1.,1.,1.,1.,1.,1.,1.,1.,1.,1.,1.,1.,
1.,1.,1.,1.,1.,1.))
REPRESENTATION_ITEM('')
);
#101=(
BOUNDED_CURVE()
B_SPLINE_CURVE(5,(#28081,#28082,#28083,#28084,#28085,#28086,#28087,#28088,
#28089,#28090,#28091,#28092,#28093,#28094,#28095,#28096,#28097,#28098,#28099,
#28100,#28101,#28102,#28103,#28104,#28105,#28106,#28107,#28108,#28109,#28110,
#28111,#28112,#28113,#28114,#28115,#28116,#28117,#28118,#28119,#28120,#28121,
#28122,#28123,#28124,#28125,#28126,#28127,#28128,#28129,#28130,#28131,#28132,
#28133,#28134,#28135,#28136,#28137,#28138,#28139,#28140,#28141,#28142,#28143,
#28144,#28145,#28146,#28147,#28148,#28149,#28150),.UNSPECIFIED.,.F.,.F.)
B_SPLINE_CURVE_WITH_KNOTS((6,1,1,1,1,1,1,1,1,1,1,1,1,1,1,1,1,1,1,1,1,1,
1,1,1,1,1,1,1,1,1,1,1,1,1,1,1,1,1,1,1,1,1,1,1,1,1,1,1,1,1,1,1,1,1,1,1,1,
1,1,1,1,1,1,1,6),(-1.,-0.984615384615383,-0.969230769230768,-0.953846153846152,
-0.938461538461537,-0.923076923076922,-0.907692307692306,-0.892307692307691,
-0.876923076923076,-0.86153846153846,-0.846153846153845,-0.83076923076923,
-0.815384615384614,-0.799999999999999,-0.784615384615384,-0.769230769230768,
-0.753846153846153,-0.738461538461538,-0.723076923076922,-0.707692307692307,
-0.692307692307692,-0.676923076923076,-0.661538461538461,-0.646153846153846,
-0.63076923076923,-0.615384615384615,-0.6,-0.584615384615384,-0.569230769230769,
-0.553846153846154,-0.538461538461538,-0.523076923076923,-0.507692307692308,
-0.492307692307692,-0.476923076923077,-0.461538461538462,-0.446153846153846,
-0.430769230769231,-0.415384615384615,-0.4,-0.384615384615385,-0.369230769230769,
-0.353846153846154,-0.338461538461538,-0.323076923076923,-0.307692307692308,
-0.292307692307692,-0.276923076923077,-0.261538461538462,-0.246153846153846,
-0.230769230769231,-0.215384615384615,-0.2,-0.184615384615385,-0.169230769230769,
-0.153846153846154,-0.138461538461538,-0.123076923076923,-0.107692307692308,
-0.0923076923076923,-0.0769230769230769,-0.0615384615384615,-0.0461538461538462,
-0.0307692307692308,-0.0153846153846154,0.),.UNSPECIFIED.)
CURVE()
GEOMETRIC_REPRESENTATION_ITEM()
RATIONAL_B_SPLINE_CURVE((1.,1.,1.,1.,1.,1.,1.,1.,1.,1.,1.,1.,1.,1.,1.,1.,
1.,1.,1.,1.,1.,1.,1.,1.,1.,1.,1.,1.,1.,1.,1.,1.,1.,1.,1.,1.,1.,1.,1.,1.,
1.,1.,1.,1.,1.,1.,1.,1.,1.,1.,1.,1.,1.,1.,1.,1.,1.,1.,1.,1.,1.,1.,1.,1.,
1.,1.,1.,1.,1.,1.))
REPRESENTATION_ITEM('')
);
#102=(
BOUNDED_CURVE()
B_SPLINE_CURVE(5,(#28297,#28298,#28299,#28300,#28301,#28302,#28303,#28304,
#28305,#28306,#28307,#28308,#28309,#28310,#28311,#28312,#28313,#28314,#28315,
#28316,#28317,#28318,#28319,#28320,#28321,#28322,#28323,#28324,#28325,#28326,
#28327,#28328,#28329,#28330,#28331,#28332,#28333,#28334,#28335,#28336,#28337,
#28338,#28339,#28340,#28341,#28342,#28343,#28344,#28345,#28346,#28347,#28348,
#28349,#28350,#28351,#28352,#28353,#28354,#28355,#28356,#28357,#28358,#28359,
#28360,#28361,#28362,#28363,#28364,#28365,#28366),.UNSPECIFIED.,.F.,.F.)
B_SPLINE_CURVE_WITH_KNOTS((6,1,1,1,1,1,1,1,1,1,1,1,1,1,1,1,1,1,1,1,1,1,
1,1,1,1,1,1,1,1,1,1,1,1,1,1,1,1,1,1,1,1,1,1,1,1,1,1,1,1,1,1,1,1,1,1,1,1,
1,1,1,1,1,1,1,6),(-1.,-0.984615384615383,-0.969230769230768,-0.953846153846152,
-0.938461538461537,-0.923076923076922,-0.907692307692306,-0.892307692307691,
-0.876923076923076,-0.86153846153846,-0.846153846153845,-0.83076923076923,
-0.815384615384614,-0.799999999999999,-0.784615384615384,-0.769230769230768,
-0.753846153846153,-0.738461538461538,-0.723076923076922,-0.707692307692307,
-0.692307692307692,-0.676923076923076,-0.661538461538461,-0.646153846153846,
-0.63076923076923,-0.615384615384615,-0.6,-0.584615384615384,-0.569230769230769,
-0.553846153846154,-0.538461538461538,-0.523076923076923,-0.507692307692308,
-0.492307692307692,-0.476923076923077,-0.461538461538462,-0.446153846153846,
-0.430769230769231,-0.415384615384615,-0.4,-0.384615384615385,-0.369230769230769,
-0.353846153846154,-0.338461538461538,-0.323076923076923,-0.307692307692308,
-0.292307692307692,-0.276923076923077,-0.261538461538462,-0.246153846153846,
-0.230769230769231,-0.215384615384615,-0.2,-0.184615384615385,-0.169230769230769,
-0.153846153846154,-0.138461538461538,-0.123076923076923,-0.107692307692308,
-0.0923076923076923,-0.0769230769230769,-0.0615384615384615,-0.0461538461538462,
-0.0307692307692308,-0.0153846153846154,0.),.UNSPECIFIED.)
CURVE()
GEOMETRIC_REPRESENTATION_ITEM()
RATIONAL_B_SPLINE_CURVE((1.,1.,1.,1.,1.,1.,1.,1.,1.,1.,1.,1.,1.,1.,1.,1.,
1.,1.,1.,1.,1.,1.,1.,1.,1.,1.,1.,1.,1.,1.,1.,1.,1.,1.,1.,1.,1.,1.,1.,1.,
1.,1.,1.,1.,1.,1.,1.,1.,1.,1.,1.,1.,1.,1.,1.,1.,1.,1.,1.,1.,1.,1.,1.,1.,
1.,1.,1.,1.,1.,1.))
REPRESENTATION_ITEM('')
);
#103=(
BOUNDED_CURVE()
B_SPLINE_CURVE(5,(#28513,#28514,#28515,#28516,#28517,#28518,#28519,#28520,
#28521,#28522,#28523,#28524,#28525,#28526,#28527,#28528,#28529,#28530,#28531,
#28532,#28533,#28534,#28535,#28536,#28537,#28538,#28539,#28540,#28541,#28542,
#28543,#28544,#28545,#28546,#28547,#28548,#28549,#28550,#28551,#28552,#28553,
#28554,#28555,#28556,#28557,#28558,#28559,#28560,#28561,#28562,#28563,#28564,
#28565,#28566,#28567,#28568,#28569,#28570,#28571,#28572,#28573,#28574,#28575,
#28576,#28577,#28578,#28579,#28580,#28581,#28582),.UNSPECIFIED.,.F.,.F.)
B_SPLINE_CURVE_WITH_KNOTS((6,1,1,1,1,1,1,1,1,1,1,1,1,1,1,1,1,1,1,1,1,1,
1,1,1,1,1,1,1,1,1,1,1,1,1,1,1,1,1,1,1,1,1,1,1,1,1,1,1,1,1,1,1,1,1,1,1,1,
1,1,1,1,1,1,1,6),(-1.,-0.984615384615383,-0.969230769230768,-0.953846153846152,
-0.938461538461537,-0.923076923076922,-0.907692307692306,-0.892307692307691,
-0.876923076923076,-0.86153846153846,-0.846153846153845,-0.83076923076923,
-0.815384615384614,-0.799999999999999,-0.784615384615384,-0.769230769230768,
-0.753846153846153,-0.738461538461538,-0.723076923076922,-0.707692307692307,
-0.692307692307692,-0.676923076923076,-0.661538461538461,-0.646153846153846,
-0.63076923076923,-0.615384615384615,-0.6,-0.584615384615384,-0.569230769230769,
-0.553846153846154,-0.538461538461538,-0.523076923076923,-0.507692307692308,
-0.492307692307692,-0.476923076923077,-0.461538461538462,-0.446153846153846,
-0.430769230769231,-0.415384615384615,-0.4,-0.384615384615385,-0.369230769230769,
-0.353846153846154,-0.338461538461538,-0.323076923076923,-0.307692307692308,
-0.292307692307692,-0.276923076923077,-0.261538461538462,-0.246153846153846,
-0.230769230769231,-0.215384615384615,-0.2,-0.184615384615385,-0.169230769230769,
-0.153846153846154,-0.138461538461538,-0.123076923076923,-0.107692307692308,
-0.0923076923076923,-0.0769230769230769,-0.0615384615384615,-0.0461538461538462,
-0.0307692307692308,-0.0153846153846154,0.),.UNSPECIFIED.)
CURVE()
GEOMETRIC_REPRESENTATION_ITEM()
RATIONAL_B_SPLINE_CURVE((1.,1.,1.,1.,1.,1.,1.,1.,1.,1.,1.,1.,1.,1.,1.,1.,
1.,1.,1.,1.,1.,1.,1.,1.,1.,1.,1.,1.,1.,1.,1.,1.,1.,1.,1.,1.,1.,1.,1.,1.,
1.,1.,1.,1.,1.,1.,1.,1.,1.,1.,1.,1.,1.,1.,1.,1.,1.,1.,1.,1.,1.,1.,1.,1.,
1.,1.,1.,1.,1.,1.))
REPRESENTATION_ITEM('')
);
#104=(
BOUNDED_CURVE()
B_SPLINE_CURVE(5,(#28729,#28730,#28731,#28732,#28733,#28734,#28735,#28736,
#28737,#28738,#28739,#28740,#28741,#28742,#28743,#28744,#28745,#28746,#28747,
#28748,#28749,#28750,#28751,#28752,#28753,#28754,#28755,#28756,#28757,#28758,
#28759,#28760,#28761,#28762,#28763,#28764,#28765,#28766,#28767,#28768,#28769,
#28770,#28771,#28772,#28773,#28774,#28775,#28776,#28777,#28778,#28779,#28780,
#28781,#28782,#28783,#28784,#28785,#28786,#28787,#28788,#28789,#28790,#28791,
#28792,#28793,#28794,#28795,#28796,#28797,#28798),.UNSPECIFIED.,.F.,.F.)
B_SPLINE_CURVE_WITH_KNOTS((6,1,1,1,1,1,1,1,1,1,1,1,1,1,1,1,1,1,1,1,1,1,
1,1,1,1,1,1,1,1,1,1,1,1,1,1,1,1,1,1,1,1,1,1,1,1,1,1,1,1,1,1,1,1,1,1,1,1,
1,1,1,1,1,1,1,6),(-1.,-0.984615384615383,-0.969230769230768,-0.953846153846152,
-0.938461538461537,-0.923076923076922,-0.907692307692306,-0.892307692307691,
-0.876923076923076,-0.86153846153846,-0.846153846153845,-0.83076923076923,
-0.815384615384614,-0.799999999999999,-0.784615384615384,-0.769230769230768,
-0.753846153846153,-0.738461538461538,-0.723076923076922,-0.707692307692307,
-0.692307692307692,-0.676923076923076,-0.661538461538461,-0.646153846153846,
-0.63076923076923,-0.615384615384615,-0.6,-0.584615384615384,-0.569230769230769,
-0.553846153846154,-0.538461538461538,-0.523076923076923,-0.507692307692308,
-0.492307692307692,-0.476923076923077,-0.461538461538462,-0.446153846153846,
-0.430769230769231,-0.415384615384615,-0.4,-0.384615384615385,-0.369230769230769,
-0.353846153846154,-0.338461538461538,-0.323076923076923,-0.307692307692308,
-0.292307692307692,-0.276923076923077,-0.261538461538462,-0.246153846153846,
-0.230769230769231,-0.215384615384615,-0.2,-0.184615384615385,-0.169230769230769,
-0.153846153846154,-0.138461538461538,-0.123076923076923,-0.107692307692308,
-0.0923076923076923,-0.0769230769230769,-0.0615384615384615,-0.0461538461538462,
-0.0307692307692308,-0.0153846153846154,0.),.UNSPECIFIED.)
CURVE()
GEOMETRIC_REPRESENTATION_ITEM()
RATIONAL_B_SPLINE_CURVE((1.,1.,1.,1.,1.,1.,1.,1.,1.,1.,1.,1.,1.,1.,1.,1.,
1.,1.,1.,1.,1.,1.,1.,1.,1.,1.,1.,1.,1.,1.,1.,1.,1.,1.,1.,1.,1.,1.,1.,1.,
1.,1.,1.,1.,1.,1.,1.,1.,1.,1.,1.,1.,1.,1.,1.,1.,1.,1.,1.,1.,1.,1.,1.,1.,
1.,1.,1.,1.,1.,1.))
REPRESENTATION_ITEM('')
);
#105=(
BOUNDED_CURVE()
B_SPLINE_CURVE(5,(#28945,#28946,#28947,#28948,#28949,#28950,#28951,#28952,
#28953,#28954,#28955,#28956,#28957,#28958,#28959,#28960,#28961,#28962,#28963,
#28964,#28965,#28966,#28967,#28968,#28969,#28970,#28971,#28972,#28973,#28974,
#28975,#28976,#28977,#28978,#28979,#28980,#28981,#28982,#28983,#28984,#28985,
#28986,#28987,#28988,#28989,#28990,#28991,#28992,#28993,#28994,#28995,#28996,
#28997,#28998,#28999,#29000,#29001,#29002,#29003,#29004,#29005,#29006,#29007,
#29008,#29009,#29010,#29011,#29012,#29013,#29014),.UNSPECIFIED.,.F.,.F.)
B_SPLINE_CURVE_WITH_KNOTS((6,1,1,1,1,1,1,1,1,1,1,1,1,1,1,1,1,1,1,1,1,1,
1,1,1,1,1,1,1,1,1,1,1,1,1,1,1,1,1,1,1,1,1,1,1,1,1,1,1,1,1,1,1,1,1,1,1,1,
1,1,1,1,1,1,1,6),(-1.,-0.984615384615383,-0.969230769230768,-0.953846153846152,
-0.938461538461537,-0.923076923076922,-0.907692307692306,-0.892307692307691,
-0.876923076923076,-0.86153846153846,-0.846153846153845,-0.83076923076923,
-0.815384615384614,-0.799999999999999,-0.784615384615384,-0.769230769230768,
-0.753846153846153,-0.738461538461538,-0.723076923076922,-0.707692307692307,
-0.692307692307692,-0.676923076923076,-0.661538461538461,-0.646153846153846,
-0.63076923076923,-0.615384615384615,-0.6,-0.584615384615384,-0.569230769230769,
-0.553846153846154,-0.538461538461538,-0.523076923076923,-0.507692307692308,
-0.492307692307692,-0.476923076923077,-0.461538461538462,-0.446153846153846,
-0.430769230769231,-0.415384615384615,-0.4,-0.384615384615385,-0.369230769230769,
-0.353846153846154,-0.338461538461538,-0.323076923076923,-0.307692307692308,
-0.292307692307692,-0.276923076923077,-0.261538461538462,-0.246153846153846,
-0.230769230769231,-0.215384615384615,-0.2,-0.184615384615385,-0.169230769230769,
-0.153846153846154,-0.138461538461538,-0.123076923076923,-0.107692307692308,
-0.0923076923076923,-0.0769230769230769,-0.0615384615384615,-0.0461538461538462,
-0.0307692307692308,-0.0153846153846154,0.),.UNSPECIFIED.)
CURVE()
GEOMETRIC_REPRESENTATION_ITEM()
RATIONAL_B_SPLINE_CURVE((1.,1.,1.,1.,1.,1.,1.,1.,1.,1.,1.,1.,1.,1.,1.,1.,
1.,1.,1.,1.,1.,1.,1.,1.,1.,1.,1.,1.,1.,1.,1.,1.,1.,1.,1.,1.,1.,1.,1.,1.,
1.,1.,1.,1.,1.,1.,1.,1.,1.,1.,1.,1.,1.,1.,1.,1.,1.,1.,1.,1.,1.,1.,1.,1.,
1.,1.,1.,1.,1.,1.))
REPRESENTATION_ITEM('')
);
#106=(
BOUNDED_CURVE()
B_SPLINE_CURVE(5,(#29161,#29162,#29163,#29164,#29165,#29166,#29167,#29168,
#29169,#29170,#29171,#29172,#29173,#29174,#29175,#29176,#29177,#29178,#29179,
#29180,#29181,#29182,#29183,#29184,#29185,#29186,#29187,#29188,#29189,#29190,
#29191,#29192,#29193,#29194,#29195,#29196,#29197,#29198,#29199,#29200,#29201,
#29202,#29203,#29204,#29205,#29206,#29207,#29208,#29209,#29210,#29211,#29212,
#29213,#29214,#29215,#29216,#29217,#29218,#29219,#29220,#29221,#29222,#29223,
#29224,#29225,#29226,#29227,#29228,#29229,#29230),.UNSPECIFIED.,.F.,.F.)
B_SPLINE_CURVE_WITH_KNOTS((6,1,1,1,1,1,1,1,1,1,1,1,1,1,1,1,1,1,1,1,1,1,
1,1,1,1,1,1,1,1,1,1,1,1,1,1,1,1,1,1,1,1,1,1,1,1,1,1,1,1,1,1,1,1,1,1,1,1,
1,1,1,1,1,1,1,6),(-1.,-0.984615384615383,-0.969230769230768,-0.953846153846152,
-0.938461538461537,-0.923076923076922,-0.907692307692306,-0.892307692307691,
-0.876923076923076,-0.86153846153846,-0.846153846153845,-0.83076923076923,
-0.815384615384614,-0.799999999999999,-0.784615384615384,-0.769230769230768,
-0.753846153846153,-0.738461538461538,-0.723076923076922,-0.707692307692307,
-0.692307692307692,-0.676923076923076,-0.661538461538461,-0.646153846153846,
-0.63076923076923,-0.615384615384615,-0.6,-0.584615384615384,-0.569230769230769,
-0.553846153846154,-0.538461538461538,-0.523076923076923,-0.507692307692308,
-0.492307692307692,-0.476923076923077,-0.461538461538462,-0.446153846153846,
-0.430769230769231,-0.415384615384615,-0.4,-0.384615384615385,-0.369230769230769,
-0.353846153846154,-0.338461538461538,-0.323076923076923,-0.307692307692308,
-0.292307692307692,-0.276923076923077,-0.261538461538462,-0.246153846153846,
-0.230769230769231,-0.215384615384615,-0.2,-0.184615384615385,-0.169230769230769,
-0.153846153846154,-0.138461538461538,-0.123076923076923,-0.107692307692308,
-0.0923076923076923,-0.0769230769230769,-0.0615384615384615,-0.0461538461538462,
-0.0307692307692308,-0.0153846153846154,0.),.UNSPECIFIED.)
CURVE()
GEOMETRIC_REPRESENTATION_ITEM()
RATIONAL_B_SPLINE_CURVE((1.,1.,1.,1.,1.,1.,1.,1.,1.,1.,1.,1.,1.,1.,1.,1.,
1.,1.,1.,1.,1.,1.,1.,1.,1.,1.,1.,1.,1.,1.,1.,1.,1.,1.,1.,1.,1.,1.,1.,1.,
1.,1.,1.,1.,1.,1.,1.,1.,1.,1.,1.,1.,1.,1.,1.,1.,1.,1.,1.,1.,1.,1.,1.,1.,
1.,1.,1.,1.,1.,1.))
REPRESENTATION_ITEM('')
);
#107=(
BOUNDED_CURVE()
B_SPLINE_CURVE(5,(#29377,#29378,#29379,#29380,#29381,#29382,#29383,#29384,
#29385,#29386,#29387,#29388,#29389,#29390,#29391,#29392,#29393,#29394,#29395,
#29396,#29397,#29398,#29399,#29400,#29401,#29402,#29403,#29404,#29405,#29406,
#29407,#29408,#29409,#29410,#29411,#29412,#29413,#29414,#29415,#29416,#29417,
#29418,#29419,#29420,#29421,#29422,#29423,#29424,#29425,#29426,#29427,#29428,
#29429,#29430,#29431,#29432,#29433,#29434,#29435,#29436,#29437,#29438,#29439,
#29440,#29441,#29442,#29443,#29444,#29445,#29446),.UNSPECIFIED.,.F.,.F.)
B_SPLINE_CURVE_WITH_KNOTS((6,1,1,1,1,1,1,1,1,1,1,1,1,1,1,1,1,1,1,1,1,1,
1,1,1,1,1,1,1,1,1,1,1,1,1,1,1,1,1,1,1,1,1,1,1,1,1,1,1,1,1,1,1,1,1,1,1,1,
1,1,1,1,1,1,1,6),(-1.,-0.984615384615383,-0.969230769230768,-0.953846153846152,
-0.938461538461537,-0.923076923076922,-0.907692307692306,-0.892307692307691,
-0.876923076923076,-0.86153846153846,-0.846153846153845,-0.83076923076923,
-0.815384615384614,-0.799999999999999,-0.784615384615384,-0.769230769230768,
-0.753846153846153,-0.738461538461538,-0.723076923076922,-0.707692307692307,
-0.692307692307692,-0.676923076923076,-0.661538461538461,-0.646153846153846,
-0.63076923076923,-0.615384615384615,-0.6,-0.584615384615384,-0.569230769230769,
-0.553846153846154,-0.538461538461538,-0.523076923076923,-0.507692307692308,
-0.492307692307692,-0.476923076923077,-0.461538461538462,-0.446153846153846,
-0.430769230769231,-0.415384615384615,-0.4,-0.384615384615385,-0.369230769230769,
-0.353846153846154,-0.338461538461538,-0.323076923076923,-0.307692307692308,
-0.292307692307692,-0.276923076923077,-0.261538461538462,-0.246153846153846,
-0.230769230769231,-0.215384615384615,-0.2,-0.184615384615385,-0.169230769230769,
-0.153846153846154,-0.138461538461538,-0.123076923076923,-0.107692307692308,
-0.0923076923076923,-0.0769230769230769,-0.0615384615384615,-0.0461538461538462,
-0.0307692307692308,-0.0153846153846154,0.),.UNSPECIFIED.)
CURVE()
GEOMETRIC_REPRESENTATION_ITEM()
RATIONAL_B_SPLINE_CURVE((1.,1.,1.,1.,1.,1.,1.,1.,1.,1.,1.,1.,1.,1.,1.,1.,
1.,1.,1.,1.,1.,1.,1.,1.,1.,1.,1.,1.,1.,1.,1.,1.,1.,1.,1.,1.,1.,1.,1.,1.,
1.,1.,1.,1.,1.,1.,1.,1.,1.,1.,1.,1.,1.,1.,1.,1.,1.,1.,1.,1.,1.,1.,1.,1.,
1.,1.,1.,1.,1.,1.))
REPRESENTATION_ITEM('')
);
#108=(
BOUNDED_CURVE()
B_SPLINE_CURVE(5,(#29593,#29594,#29595,#29596,#29597,#29598,#29599,#29600,
#29601,#29602,#29603,#29604,#29605,#29606,#29607,#29608,#29609,#29610,#29611,
#29612,#29613,#29614,#29615,#29616,#29617,#29618,#29619,#29620,#29621,#29622,
#29623,#29624,#29625,#29626,#29627,#29628,#29629,#29630,#29631,#29632,#29633,
#29634,#29635,#29636,#29637,#29638,#29639,#29640,#29641,#29642,#29643,#29644,
#29645,#29646,#29647,#29648,#29649,#29650,#29651,#29652,#29653,#29654,#29655,
#29656,#29657,#29658,#29659,#29660,#29661,#29662),.UNSPECIFIED.,.F.,.F.)
B_SPLINE_CURVE_WITH_KNOTS((6,1,1,1,1,1,1,1,1,1,1,1,1,1,1,1,1,1,1,1,1,1,
1,1,1,1,1,1,1,1,1,1,1,1,1,1,1,1,1,1,1,1,1,1,1,1,1,1,1,1,1,1,1,1,1,1,1,1,
1,1,1,1,1,1,1,6),(-1.,-0.984615384615383,-0.969230769230768,-0.953846153846152,
-0.938461538461537,-0.923076923076922,-0.907692307692306,-0.892307692307691,
-0.876923076923076,-0.86153846153846,-0.846153846153845,-0.83076923076923,
-0.815384615384614,-0.799999999999999,-0.784615384615384,-0.769230769230768,
-0.753846153846153,-0.738461538461538,-0.723076923076922,-0.707692307692307,
-0.692307692307692,-0.676923076923076,-0.661538461538461,-0.646153846153846,
-0.63076923076923,-0.615384615384615,-0.6,-0.584615384615384,-0.569230769230769,
-0.553846153846154,-0.538461538461538,-0.523076923076923,-0.507692307692308,
-0.492307692307692,-0.476923076923077,-0.461538461538462,-0.446153846153846,
-0.430769230769231,-0.415384615384615,-0.4,-0.384615384615385,-0.369230769230769,
-0.353846153846154,-0.338461538461538,-0.323076923076923,-0.307692307692308,
-0.292307692307692,-0.276923076923077,-0.261538461538462,-0.246153846153846,
-0.230769230769231,-0.215384615384615,-0.2,-0.184615384615385,-0.169230769230769,
-0.153846153846154,-0.138461538461538,-0.123076923076923,-0.107692307692308,
-0.0923076923076923,-0.0769230769230769,-0.0615384615384615,-0.0461538461538462,
-0.0307692307692308,-0.0153846153846154,0.),.UNSPECIFIED.)
CURVE()
GEOMETRIC_REPRESENTATION_ITEM()
RATIONAL_B_SPLINE_CURVE((1.,1.,1.,1.,1.,1.,1.,1.,1.,1.,1.,1.,1.,1.,1.,1.,
1.,1.,1.,1.,1.,1.,1.,1.,1.,1.,1.,1.,1.,1.,1.,1.,1.,1.,1.,1.,1.,1.,1.,1.,
1.,1.,1.,1.,1.,1.,1.,1.,1.,1.,1.,1.,1.,1.,1.,1.,1.,1.,1.,1.,1.,1.,1.,1.,
1.,1.,1.,1.,1.,1.))
REPRESENTATION_ITEM('')
);
#109=(
BOUNDED_CURVE()
B_SPLINE_CURVE(5,(#29809,#29810,#29811,#29812,#29813,#29814,#29815,#29816,
#29817,#29818,#29819,#29820,#29821,#29822,#29823,#29824,#29825,#29826,#29827,
#29828,#29829,#29830,#29831,#29832,#29833,#29834,#29835,#29836,#29837,#29838,
#29839,#29840,#29841,#29842,#29843,#29844,#29845,#29846,#29847,#29848,#29849,
#29850,#29851,#29852,#29853,#29854,#29855,#29856,#29857,#29858,#29859,#29860,
#29861,#29862,#29863,#29864,#29865,#29866,#29867,#29868,#29869,#29870,#29871,
#29872,#29873,#29874,#29875,#29876,#29877,#29878),.UNSPECIFIED.,.F.,.F.)
B_SPLINE_CURVE_WITH_KNOTS((6,1,1,1,1,1,1,1,1,1,1,1,1,1,1,1,1,1,1,1,1,1,
1,1,1,1,1,1,1,1,1,1,1,1,1,1,1,1,1,1,1,1,1,1,1,1,1,1,1,1,1,1,1,1,1,1,1,1,
1,1,1,1,1,1,1,6),(-1.,-0.984615384615383,-0.969230769230768,-0.953846153846152,
-0.938461538461537,-0.923076923076922,-0.907692307692306,-0.892307692307691,
-0.876923076923076,-0.86153846153846,-0.846153846153845,-0.83076923076923,
-0.815384615384614,-0.799999999999999,-0.784615384615384,-0.769230769230768,
-0.753846153846153,-0.738461538461538,-0.723076923076922,-0.707692307692307,
-0.692307692307692,-0.676923076923076,-0.661538461538461,-0.646153846153846,
-0.63076923076923,-0.615384615384615,-0.6,-0.584615384615384,-0.569230769230769,
-0.553846153846154,-0.538461538461538,-0.523076923076923,-0.507692307692308,
-0.492307692307692,-0.476923076923077,-0.461538461538462,-0.446153846153846,
-0.430769230769231,-0.415384615384615,-0.4,-0.384615384615385,-0.369230769230769,
-0.353846153846154,-0.338461538461538,-0.323076923076923,-0.307692307692308,
-0.292307692307692,-0.276923076923077,-0.261538461538462,-0.246153846153846,
-0.230769230769231,-0.215384615384615,-0.2,-0.184615384615385,-0.169230769230769,
-0.153846153846154,-0.138461538461538,-0.123076923076923,-0.107692307692308,
-0.0923076923076923,-0.0769230769230769,-0.0615384615384615,-0.0461538461538462,
-0.0307692307692308,-0.0153846153846154,0.),.UNSPECIFIED.)
CURVE()
GEOMETRIC_REPRESENTATION_ITEM()
RATIONAL_B_SPLINE_CURVE((1.,1.,1.,1.,1.,1.,1.,1.,1.,1.,1.,1.,1.,1.,1.,1.,
1.,1.,1.,1.,1.,1.,1.,1.,1.,1.,1.,1.,1.,1.,1.,1.,1.,1.,1.,1.,1.,1.,1.,1.,
1.,1.,1.,1.,1.,1.,1.,1.,1.,1.,1.,1.,1.,1.,1.,1.,1.,1.,1.,1.,1.,1.,1.,1.,
1.,1.,1.,1.,1.,1.))
REPRESENTATION_ITEM('')
);
#110=(
BOUNDED_CURVE()
B_SPLINE_CURVE(5,(#30025,#30026,#30027,#30028,#30029,#30030,#30031,#30032,
#30033,#30034,#30035,#30036,#30037,#30038,#30039,#30040,#30041,#30042,#30043,
#30044,#30045,#30046,#30047,#30048,#30049,#30050,#30051,#30052,#30053,#30054,
#30055,#30056,#30057,#30058,#30059,#30060,#30061,#30062,#30063,#30064,#30065,
#30066,#30067,#30068,#30069,#30070,#30071,#30072,#30073,#30074,#30075,#30076,
#30077,#30078,#30079,#30080,#30081,#30082,#30083,#30084,#30085,#30086,#30087,
#30088,#30089,#30090,#30091,#30092,#30093,#30094),.UNSPECIFIED.,.F.,.F.)
B_SPLINE_CURVE_WITH_KNOTS((6,1,1,1,1,1,1,1,1,1,1,1,1,1,1,1,1,1,1,1,1,1,
1,1,1,1,1,1,1,1,1,1,1,1,1,1,1,1,1,1,1,1,1,1,1,1,1,1,1,1,1,1,1,1,1,1,1,1,
1,1,1,1,1,1,1,6),(-1.,-0.984615384615383,-0.969230769230768,-0.953846153846152,
-0.938461538461537,-0.923076923076922,-0.907692307692306,-0.892307692307691,
-0.876923076923076,-0.86153846153846,-0.846153846153845,-0.83076923076923,
-0.815384615384614,-0.799999999999999,-0.784615384615384,-0.769230769230768,
-0.753846153846153,-0.738461538461538,-0.723076923076922,-0.707692307692307,
-0.692307692307692,-0.676923076923076,-0.661538461538461,-0.646153846153846,
-0.63076923076923,-0.615384615384615,-0.6,-0.584615384615384,-0.569230769230769,
-0.553846153846154,-0.538461538461538,-0.523076923076923,-0.507692307692308,
-0.492307692307692,-0.476923076923077,-0.461538461538462,-0.446153846153846,
-0.430769230769231,-0.415384615384615,-0.4,-0.384615384615385,-0.369230769230769,
-0.353846153846154,-0.338461538461538,-0.323076923076923,-0.307692307692308,
-0.292307692307692,-0.276923076923077,-0.261538461538462,-0.246153846153846,
-0.230769230769231,-0.215384615384615,-0.2,-0.184615384615385,-0.169230769230769,
-0.153846153846154,-0.138461538461538,-0.123076923076923,-0.107692307692308,
-0.0923076923076923,-0.0769230769230769,-0.0615384615384615,-0.0461538461538462,
-0.0307692307692308,-0.0153846153846154,0.),.UNSPECIFIED.)
CURVE()
GEOMETRIC_REPRESENTATION_ITEM()
RATIONAL_B_SPLINE_CURVE((1.,1.,1.,1.,1.,1.,1.,1.,1.,1.,1.,1.,1.,1.,1.,1.,
1.,1.,1.,1.,1.,1.,1.,1.,1.,1.,1.,1.,1.,1.,1.,1.,1.,1.,1.,1.,1.,1.,1.,1.,
1.,1.,1.,1.,1.,1.,1.,1.,1.,1.,1.,1.,1.,1.,1.,1.,1.,1.,1.,1.,1.,1.,1.,1.,
1.,1.,1.,1.,1.,1.))
REPRESENTATION_ITEM('')
);
#111=(
BOUNDED_CURVE()
B_SPLINE_CURVE(5,(#30241,#30242,#30243,#30244,#30245,#30246,#30247,#30248,
#30249,#30250,#30251,#30252,#30253,#30254,#30255,#30256,#30257,#30258,#30259,
#30260,#30261,#30262,#30263,#30264,#30265,#30266,#30267,#30268,#30269,#30270,
#30271,#30272,#30273,#30274,#30275,#30276,#30277,#30278,#30279,#30280,#30281,
#30282,#30283,#30284,#30285,#30286,#30287,#30288,#30289,#30290,#30291,#30292,
#30293,#30294,#30295,#30296,#30297,#30298,#30299,#30300,#30301,#30302,#30303,
#30304,#30305,#30306,#30307,#30308,#30309,#30310),.UNSPECIFIED.,.F.,.F.)
B_SPLINE_CURVE_WITH_KNOTS((6,1,1,1,1,1,1,1,1,1,1,1,1,1,1,1,1,1,1,1,1,1,
1,1,1,1,1,1,1,1,1,1,1,1,1,1,1,1,1,1,1,1,1,1,1,1,1,1,1,1,1,1,1,1,1,1,1,1,
1,1,1,1,1,1,1,6),(-1.,-0.984615384615383,-0.969230769230768,-0.953846153846152,
-0.938461538461537,-0.923076923076922,-0.907692307692306,-0.892307692307691,
-0.876923076923076,-0.86153846153846,-0.846153846153845,-0.83076923076923,
-0.815384615384614,-0.799999999999999,-0.784615384615384,-0.769230769230768,
-0.753846153846153,-0.738461538461538,-0.723076923076922,-0.707692307692307,
-0.692307692307692,-0.676923076923076,-0.661538461538461,-0.646153846153846,
-0.63076923076923,-0.615384615384615,-0.6,-0.584615384615384,-0.569230769230769,
-0.553846153846154,-0.538461538461538,-0.523076923076923,-0.507692307692308,
-0.492307692307692,-0.476923076923077,-0.461538461538462,-0.446153846153846,
-0.430769230769231,-0.415384615384615,-0.4,-0.384615384615385,-0.369230769230769,
-0.353846153846154,-0.338461538461538,-0.323076923076923,-0.307692307692308,
-0.292307692307692,-0.276923076923077,-0.261538461538462,-0.246153846153846,
-0.230769230769231,-0.215384615384615,-0.2,-0.184615384615385,-0.169230769230769,
-0.153846153846154,-0.138461538461538,-0.123076923076923,-0.107692307692308,
-0.0923076923076923,-0.0769230769230769,-0.0615384615384615,-0.0461538461538462,
-0.0307692307692308,-0.0153846153846154,0.),.UNSPECIFIED.)
CURVE()
GEOMETRIC_REPRESENTATION_ITEM()
RATIONAL_B_SPLINE_CURVE((1.,1.,1.,1.,1.,1.,1.,1.,1.,1.,1.,1.,1.,1.,1.,1.,
1.,1.,1.,1.,1.,1.,1.,1.,1.,1.,1.,1.,1.,1.,1.,1.,1.,1.,1.,1.,1.,1.,1.,1.,
1.,1.,1.,1.,1.,1.,1.,1.,1.,1.,1.,1.,1.,1.,1.,1.,1.,1.,1.,1.,1.,1.,1.,1.,
1.,1.,1.,1.,1.,1.))
REPRESENTATION_ITEM('')
);
#112=(
BOUNDED_CURVE()
B_SPLINE_CURVE(5,(#30457,#30458,#30459,#30460,#30461,#30462,#30463,#30464,
#30465,#30466,#30467,#30468,#30469,#30470,#30471,#30472,#30473,#30474,#30475,
#30476,#30477,#30478,#30479,#30480,#30481,#30482,#30483,#30484,#30485,#30486,
#30487,#30488,#30489,#30490,#30491,#30492,#30493,#30494,#30495,#30496,#30497,
#30498,#30499,#30500,#30501,#30502,#30503,#30504,#30505,#30506,#30507,#30508,
#30509,#30510,#30511,#30512,#30513,#30514,#30515,#30516,#30517,#30518,#30519,
#30520,#30521,#30522,#30523,#30524,#30525,#30526),.UNSPECIFIED.,.F.,.F.)
B_SPLINE_CURVE_WITH_KNOTS((6,1,1,1,1,1,1,1,1,1,1,1,1,1,1,1,1,1,1,1,1,1,
1,1,1,1,1,1,1,1,1,1,1,1,1,1,1,1,1,1,1,1,1,1,1,1,1,1,1,1,1,1,1,1,1,1,1,1,
1,1,1,1,1,1,1,6),(-1.,-0.984615384615383,-0.969230769230768,-0.953846153846152,
-0.938461538461537,-0.923076923076922,-0.907692307692306,-0.892307692307691,
-0.876923076923076,-0.86153846153846,-0.846153846153845,-0.83076923076923,
-0.815384615384614,-0.799999999999999,-0.784615384615384,-0.769230769230768,
-0.753846153846153,-0.738461538461538,-0.723076923076922,-0.707692307692307,
-0.692307692307692,-0.676923076923076,-0.661538461538461,-0.646153846153846,
-0.63076923076923,-0.615384615384615,-0.6,-0.584615384615384,-0.569230769230769,
-0.553846153846154,-0.538461538461538,-0.523076923076923,-0.507692307692308,
-0.492307692307692,-0.476923076923077,-0.461538461538462,-0.446153846153846,
-0.430769230769231,-0.415384615384615,-0.4,-0.384615384615385,-0.369230769230769,
-0.353846153846154,-0.338461538461538,-0.323076923076923,-0.307692307692308,
-0.292307692307692,-0.276923076923077,-0.261538461538462,-0.246153846153846,
-0.230769230769231,-0.215384615384615,-0.2,-0.184615384615385,-0.169230769230769,
-0.153846153846154,-0.138461538461538,-0.123076923076923,-0.107692307692308,
-0.0923076923076923,-0.0769230769230769,-0.0615384615384615,-0.0461538461538462,
-0.0307692307692308,-0.0153846153846154,0.),.UNSPECIFIED.)
CURVE()
GEOMETRIC_REPRESENTATION_ITEM()
RATIONAL_B_SPLINE_CURVE((1.,1.,1.,1.,1.,1.,1.,1.,1.,1.,1.,1.,1.,1.,1.,1.,
1.,1.,1.,1.,1.,1.,1.,1.,1.,1.,1.,1.,1.,1.,1.,1.,1.,1.,1.,1.,1.,1.,1.,1.,
1.,1.,1.,1.,1.,1.,1.,1.,1.,1.,1.,1.,1.,1.,1.,1.,1.,1.,1.,1.,1.,1.,1.,1.,
1.,1.,1.,1.,1.,1.))
REPRESENTATION_ITEM('')
);
#113=(
BOUNDED_CURVE()
B_SPLINE_CURVE(5,(#30673,#30674,#30675,#30676,#30677,#30678,#30679,#30680,
#30681,#30682,#30683,#30684,#30685,#30686,#30687,#30688,#30689,#30690,#30691,
#30692,#30693,#30694,#30695,#30696,#30697,#30698,#30699,#30700,#30701,#30702,
#30703,#30704,#30705,#30706,#30707,#30708,#30709,#30710,#30711,#30712,#30713,
#30714,#30715,#30716,#30717,#30718,#30719,#30720,#30721,#30722,#30723,#30724,
#30725,#30726,#30727,#30728,#30729,#30730,#30731,#30732,#30733,#30734,#30735,
#30736,#30737,#30738,#30739,#30740,#30741,#30742),.UNSPECIFIED.,.F.,.F.)
B_SPLINE_CURVE_WITH_KNOTS((6,1,1,1,1,1,1,1,1,1,1,1,1,1,1,1,1,1,1,1,1,1,
1,1,1,1,1,1,1,1,1,1,1,1,1,1,1,1,1,1,1,1,1,1,1,1,1,1,1,1,1,1,1,1,1,1,1,1,
1,1,1,1,1,1,1,6),(-1.,-0.984615384615383,-0.969230769230768,-0.953846153846152,
-0.938461538461537,-0.923076923076922,-0.907692307692306,-0.892307692307691,
-0.876923076923076,-0.86153846153846,-0.846153846153845,-0.83076923076923,
-0.815384615384614,-0.799999999999999,-0.784615384615384,-0.769230769230768,
-0.753846153846153,-0.738461538461538,-0.723076923076922,-0.707692307692307,
-0.692307692307692,-0.676923076923076,-0.661538461538461,-0.646153846153846,
-0.63076923076923,-0.615384615384615,-0.6,-0.584615384615384,-0.569230769230769,
-0.553846153846154,-0.538461538461538,-0.523076923076923,-0.507692307692308,
-0.492307692307692,-0.476923076923077,-0.461538461538462,-0.446153846153846,
-0.430769230769231,-0.415384615384615,-0.4,-0.384615384615385,-0.369230769230769,
-0.353846153846154,-0.338461538461538,-0.323076923076923,-0.307692307692308,
-0.292307692307692,-0.276923076923077,-0.261538461538462,-0.246153846153846,
-0.230769230769231,-0.215384615384615,-0.2,-0.184615384615385,-0.169230769230769,
-0.153846153846154,-0.138461538461538,-0.123076923076923,-0.107692307692308,
-0.0923076923076923,-0.0769230769230769,-0.0615384615384615,-0.0461538461538462,
-0.0307692307692308,-0.0153846153846154,0.),.UNSPECIFIED.)
CURVE()
GEOMETRIC_REPRESENTATION_ITEM()
RATIONAL_B_SPLINE_CURVE((1.,1.,1.,1.,1.,1.,1.,1.,1.,1.,1.,1.,1.,1.,1.,1.,
1.,1.,1.,1.,1.,1.,1.,1.,1.,1.,1.,1.,1.,1.,1.,1.,1.,1.,1.,1.,1.,1.,1.,1.,
1.,1.,1.,1.,1.,1.,1.,1.,1.,1.,1.,1.,1.,1.,1.,1.,1.,1.,1.,1.,1.,1.,1.,1.,
1.,1.,1.,1.,1.,1.))
REPRESENTATION_ITEM('')
);
#114=(
BOUNDED_CURVE()
B_SPLINE_CURVE(5,(#30889,#30890,#30891,#30892,#30893,#30894,#30895,#30896,
#30897,#30898,#30899,#30900,#30901,#30902,#30903,#30904,#30905,#30906,#30907,
#30908,#30909,#30910,#30911,#30912,#30913,#30914,#30915,#30916,#30917,#30918,
#30919,#30920,#30921,#30922,#30923,#30924,#30925,#30926,#30927,#30928,#30929,
#30930,#30931,#30932,#30933,#30934,#30935,#30936,#30937,#30938,#30939,#30940,
#30941,#30942,#30943,#30944,#30945,#30946,#30947,#30948,#30949,#30950,#30951,
#30952,#30953,#30954,#30955,#30956,#30957,#30958),.UNSPECIFIED.,.F.,.F.)
B_SPLINE_CURVE_WITH_KNOTS((6,1,1,1,1,1,1,1,1,1,1,1,1,1,1,1,1,1,1,1,1,1,
1,1,1,1,1,1,1,1,1,1,1,1,1,1,1,1,1,1,1,1,1,1,1,1,1,1,1,1,1,1,1,1,1,1,1,1,
1,1,1,1,1,1,1,6),(-1.,-0.984615384615383,-0.969230769230768,-0.953846153846152,
-0.938461538461537,-0.923076923076922,-0.907692307692306,-0.892307692307691,
-0.876923076923076,-0.86153846153846,-0.846153846153845,-0.83076923076923,
-0.815384615384614,-0.799999999999999,-0.784615384615384,-0.769230769230768,
-0.753846153846153,-0.738461538461538,-0.723076923076922,-0.707692307692307,
-0.692307692307692,-0.676923076923076,-0.661538461538461,-0.646153846153846,
-0.63076923076923,-0.615384615384615,-0.6,-0.584615384615384,-0.569230769230769,
-0.553846153846154,-0.538461538461538,-0.523076923076923,-0.507692307692308,
-0.492307692307692,-0.476923076923077,-0.461538461538462,-0.446153846153846,
-0.430769230769231,-0.415384615384615,-0.4,-0.384615384615385,-0.369230769230769,
-0.353846153846154,-0.338461538461538,-0.323076923076923,-0.307692307692308,
-0.292307692307692,-0.276923076923077,-0.261538461538462,-0.246153846153846,
-0.230769230769231,-0.215384615384615,-0.2,-0.184615384615385,-0.169230769230769,
-0.153846153846154,-0.138461538461538,-0.123076923076923,-0.107692307692308,
-0.0923076923076923,-0.0769230769230769,-0.0615384615384615,-0.0461538461538462,
-0.0307692307692308,-0.0153846153846154,0.),.UNSPECIFIED.)
CURVE()
GEOMETRIC_REPRESENTATION_ITEM()
RATIONAL_B_SPLINE_CURVE((1.,1.,1.,1.,1.,1.,1.,1.,1.,1.,1.,1.,1.,1.,1.,1.,
1.,1.,1.,1.,1.,1.,1.,1.,1.,1.,1.,1.,1.,1.,1.,1.,1.,1.,1.,1.,1.,1.,1.,1.,
1.,1.,1.,1.,1.,1.,1.,1.,1.,1.,1.,1.,1.,1.,1.,1.,1.,1.,1.,1.,1.,1.,1.,1.,
1.,1.,1.,1.,1.,1.))
REPRESENTATION_ITEM('')
);
#115=(
BOUNDED_CURVE()
B_SPLINE_CURVE(5,(#31105,#31106,#31107,#31108,#31109,#31110,#31111,#31112,
#31113,#31114,#31115,#31116,#31117,#31118,#31119,#31120,#31121,#31122,#31123,
#31124,#31125,#31126,#31127,#31128,#31129,#31130,#31131,#31132,#31133,#31134,
#31135,#31136,#31137,#31138,#31139,#31140,#31141,#31142,#31143,#31144,#31145,
#31146,#31147,#31148,#31149,#31150,#31151,#31152,#31153,#31154,#31155,#31156,
#31157,#31158,#31159,#31160,#31161,#31162,#31163,#31164,#31165,#31166,#31167,
#31168,#31169,#31170,#31171,#31172,#31173,#31174),.UNSPECIFIED.,.F.,.F.)
B_SPLINE_CURVE_WITH_KNOTS((6,1,1,1,1,1,1,1,1,1,1,1,1,1,1,1,1,1,1,1,1,1,
1,1,1,1,1,1,1,1,1,1,1,1,1,1,1,1,1,1,1,1,1,1,1,1,1,1,1,1,1,1,1,1,1,1,1,1,
1,1,1,1,1,1,1,6),(-1.,-0.984615384615383,-0.969230769230768,-0.953846153846152,
-0.938461538461537,-0.923076923076922,-0.907692307692306,-0.892307692307691,
-0.876923076923076,-0.86153846153846,-0.846153846153845,-0.83076923076923,
-0.815384615384614,-0.799999999999999,-0.784615384615384,-0.769230769230768,
-0.753846153846153,-0.738461538461538,-0.723076923076922,-0.707692307692307,
-0.692307692307692,-0.676923076923076,-0.661538461538461,-0.646153846153846,
-0.63076923076923,-0.615384615384615,-0.6,-0.584615384615384,-0.569230769230769,
-0.553846153846154,-0.538461538461538,-0.523076923076923,-0.507692307692308,
-0.492307692307692,-0.476923076923077,-0.461538461538462,-0.446153846153846,
-0.430769230769231,-0.415384615384615,-0.4,-0.384615384615385,-0.369230769230769,
-0.353846153846154,-0.338461538461538,-0.323076923076923,-0.307692307692308,
-0.292307692307692,-0.276923076923077,-0.261538461538462,-0.246153846153846,
-0.230769230769231,-0.215384615384615,-0.2,-0.184615384615385,-0.169230769230769,
-0.153846153846154,-0.138461538461538,-0.123076923076923,-0.107692307692308,
-0.0923076923076923,-0.0769230769230769,-0.0615384615384615,-0.0461538461538462,
-0.0307692307692308,-0.0153846153846154,0.),.UNSPECIFIED.)
CURVE()
GEOMETRIC_REPRESENTATION_ITEM()
RATIONAL_B_SPLINE_CURVE((1.,1.,1.,1.,1.,1.,1.,1.,1.,1.,1.,1.,1.,1.,1.,1.,
1.,1.,1.,1.,1.,1.,1.,1.,1.,1.,1.,1.,1.,1.,1.,1.,1.,1.,1.,1.,1.,1.,1.,1.,
1.,1.,1.,1.,1.,1.,1.,1.,1.,1.,1.,1.,1.,1.,1.,1.,1.,1.,1.,1.,1.,1.,1.,1.,
1.,1.,1.,1.,1.,1.))
REPRESENTATION_ITEM('')
);
#116=(
BOUNDED_CURVE()
B_SPLINE_CURVE(5,(#31321,#31322,#31323,#31324,#31325,#31326,#31327,#31328,
#31329,#31330,#31331,#31332,#31333,#31334,#31335,#31336,#31337,#31338,#31339,
#31340,#31341,#31342,#31343,#31344,#31345,#31346,#31347,#31348,#31349,#31350,
#31351,#31352,#31353,#31354,#31355,#31356,#31357,#31358,#31359,#31360,#31361,
#31362,#31363,#31364,#31365,#31366,#31367,#31368,#31369,#31370,#31371,#31372,
#31373,#31374,#31375,#31376,#31377,#31378,#31379,#31380,#31381,#31382,#31383,
#31384,#31385,#31386,#31387,#31388,#31389,#31390),.UNSPECIFIED.,.F.,.F.)
B_SPLINE_CURVE_WITH_KNOTS((6,1,1,1,1,1,1,1,1,1,1,1,1,1,1,1,1,1,1,1,1,1,
1,1,1,1,1,1,1,1,1,1,1,1,1,1,1,1,1,1,1,1,1,1,1,1,1,1,1,1,1,1,1,1,1,1,1,1,
1,1,1,1,1,1,1,6),(-1.,-0.984615384615383,-0.969230769230768,-0.953846153846152,
-0.938461538461537,-0.923076923076922,-0.907692307692306,-0.892307692307691,
-0.876923076923076,-0.86153846153846,-0.846153846153845,-0.83076923076923,
-0.815384615384614,-0.799999999999999,-0.784615384615384,-0.769230769230768,
-0.753846153846153,-0.738461538461538,-0.723076923076922,-0.707692307692307,
-0.692307692307692,-0.676923076923076,-0.661538461538461,-0.646153846153846,
-0.63076923076923,-0.615384615384615,-0.6,-0.584615384615384,-0.569230769230769,
-0.553846153846154,-0.538461538461538,-0.523076923076923,-0.507692307692308,
-0.492307692307692,-0.476923076923077,-0.461538461538462,-0.446153846153846,
-0.430769230769231,-0.415384615384615,-0.4,-0.384615384615385,-0.369230769230769,
-0.353846153846154,-0.338461538461538,-0.323076923076923,-0.307692307692308,
-0.292307692307692,-0.276923076923077,-0.261538461538462,-0.246153846153846,
-0.230769230769231,-0.215384615384615,-0.2,-0.184615384615385,-0.169230769230769,
-0.153846153846154,-0.138461538461538,-0.123076923076923,-0.107692307692308,
-0.0923076923076923,-0.0769230769230769,-0.0615384615384615,-0.0461538461538462,
-0.0307692307692308,-0.0153846153846154,0.),.UNSPECIFIED.)
CURVE()
GEOMETRIC_REPRESENTATION_ITEM()
RATIONAL_B_SPLINE_CURVE((1.,1.,1.,1.,1.,1.,1.,1.,1.,1.,1.,1.,1.,1.,1.,1.,
1.,1.,1.,1.,1.,1.,1.,1.,1.,1.,1.,1.,1.,1.,1.,1.,1.,1.,1.,1.,1.,1.,1.,1.,
1.,1.,1.,1.,1.,1.,1.,1.,1.,1.,1.,1.,1.,1.,1.,1.,1.,1.,1.,1.,1.,1.,1.,1.,
1.,1.,1.,1.,1.,1.))
REPRESENTATION_ITEM('')
);
#117=(
BOUNDED_CURVE()
B_SPLINE_CURVE(5,(#31537,#31538,#31539,#31540,#31541,#31542,#31543,#31544,
#31545,#31546,#31547,#31548,#31549,#31550,#31551,#31552,#31553,#31554,#31555,
#31556,#31557,#31558,#31559,#31560,#31561,#31562,#31563,#31564,#31565,#31566,
#31567,#31568,#31569,#31570,#31571,#31572,#31573,#31574,#31575,#31576,#31577,
#31578,#31579,#31580,#31581,#31582,#31583,#31584,#31585,#31586,#31587,#31588,
#31589,#31590,#31591,#31592,#31593,#31594,#31595,#31596,#31597,#31598,#31599,
#31600,#31601,#31602,#31603,#31604,#31605,#31606),.UNSPECIFIED.,.F.,.F.)
B_SPLINE_CURVE_WITH_KNOTS((6,1,1,1,1,1,1,1,1,1,1,1,1,1,1,1,1,1,1,1,1,1,
1,1,1,1,1,1,1,1,1,1,1,1,1,1,1,1,1,1,1,1,1,1,1,1,1,1,1,1,1,1,1,1,1,1,1,1,
1,1,1,1,1,1,1,6),(-1.,-0.984615384615383,-0.969230769230768,-0.953846153846152,
-0.938461538461537,-0.923076923076922,-0.907692307692306,-0.892307692307691,
-0.876923076923076,-0.86153846153846,-0.846153846153845,-0.83076923076923,
-0.815384615384614,-0.799999999999999,-0.784615384615384,-0.769230769230768,
-0.753846153846153,-0.738461538461538,-0.723076923076922,-0.707692307692307,
-0.692307692307692,-0.676923076923076,-0.661538461538461,-0.646153846153846,
-0.63076923076923,-0.615384615384615,-0.6,-0.584615384615384,-0.569230769230769,
-0.553846153846154,-0.538461538461538,-0.523076923076923,-0.507692307692308,
-0.492307692307692,-0.476923076923077,-0.461538461538462,-0.446153846153846,
-0.430769230769231,-0.415384615384615,-0.4,-0.384615384615385,-0.369230769230769,
-0.353846153846154,-0.338461538461538,-0.323076923076923,-0.307692307692308,
-0.292307692307692,-0.276923076923077,-0.261538461538462,-0.246153846153846,
-0.230769230769231,-0.215384615384615,-0.2,-0.184615384615385,-0.169230769230769,
-0.153846153846154,-0.138461538461538,-0.123076923076923,-0.107692307692308,
-0.0923076923076923,-0.0769230769230769,-0.0615384615384615,-0.0461538461538462,
-0.0307692307692308,-0.0153846153846154,0.),.UNSPECIFIED.)
CURVE()
GEOMETRIC_REPRESENTATION_ITEM()
RATIONAL_B_SPLINE_CURVE((1.,1.,1.,1.,1.,1.,1.,1.,1.,1.,1.,1.,1.,1.,1.,1.,
1.,1.,1.,1.,1.,1.,1.,1.,1.,1.,1.,1.,1.,1.,1.,1.,1.,1.,1.,1.,1.,1.,1.,1.,
1.,1.,1.,1.,1.,1.,1.,1.,1.,1.,1.,1.,1.,1.,1.,1.,1.,1.,1.,1.,1.,1.,1.,1.,
1.,1.,1.,1.,1.,1.))
REPRESENTATION_ITEM('')
);
#118=(
BOUNDED_CURVE()
B_SPLINE_CURVE(5,(#31753,#31754,#31755,#31756,#31757,#31758,#31759,#31760,
#31761,#31762,#31763,#31764,#31765,#31766,#31767,#31768,#31769,#31770,#31771,
#31772,#31773,#31774,#31775,#31776,#31777,#31778,#31779,#31780,#31781,#31782,
#31783,#31784,#31785,#31786,#31787,#31788,#31789,#31790,#31791,#31792,#31793,
#31794,#31795,#31796,#31797,#31798,#31799,#31800,#31801,#31802,#31803,#31804,
#31805,#31806,#31807,#31808,#31809,#31810,#31811,#31812,#31813,#31814,#31815,
#31816,#31817,#31818,#31819,#31820,#31821,#31822),.UNSPECIFIED.,.F.,.F.)
B_SPLINE_CURVE_WITH_KNOTS((6,1,1,1,1,1,1,1,1,1,1,1,1,1,1,1,1,1,1,1,1,1,
1,1,1,1,1,1,1,1,1,1,1,1,1,1,1,1,1,1,1,1,1,1,1,1,1,1,1,1,1,1,1,1,1,1,1,1,
1,1,1,1,1,1,1,6),(-1.,-0.984615384615383,-0.969230769230768,-0.953846153846152,
-0.938461538461537,-0.923076923076922,-0.907692307692306,-0.892307692307691,
-0.876923076923076,-0.86153846153846,-0.846153846153845,-0.83076923076923,
-0.815384615384614,-0.799999999999999,-0.784615384615384,-0.769230769230768,
-0.753846153846153,-0.738461538461538,-0.723076923076922,-0.707692307692307,
-0.692307692307692,-0.676923076923076,-0.661538461538461,-0.646153846153846,
-0.63076923076923,-0.615384615384615,-0.6,-0.584615384615384,-0.569230769230769,
-0.553846153846154,-0.538461538461538,-0.523076923076923,-0.507692307692308,
-0.492307692307692,-0.476923076923077,-0.461538461538462,-0.446153846153846,
-0.430769230769231,-0.415384615384615,-0.4,-0.384615384615385,-0.369230769230769,
-0.353846153846154,-0.338461538461538,-0.323076923076923,-0.307692307692308,
-0.292307692307692,-0.276923076923077,-0.261538461538462,-0.246153846153846,
-0.230769230769231,-0.215384615384615,-0.2,-0.184615384615385,-0.169230769230769,
-0.153846153846154,-0.138461538461538,-0.123076923076923,-0.107692307692308,
-0.0923076923076923,-0.0769230769230769,-0.0615384615384615,-0.0461538461538462,
-0.0307692307692308,-0.0153846153846154,0.),.UNSPECIFIED.)
CURVE()
GEOMETRIC_REPRESENTATION_ITEM()
RATIONAL_B_SPLINE_CURVE((1.,1.,1.,1.,1.,1.,1.,1.,1.,1.,1.,1.,1.,1.,1.,1.,
1.,1.,1.,1.,1.,1.,1.,1.,1.,1.,1.,1.,1.,1.,1.,1.,1.,1.,1.,1.,1.,1.,1.,1.,
1.,1.,1.,1.,1.,1.,1.,1.,1.,1.,1.,1.,1.,1.,1.,1.,1.,1.,1.,1.,1.,1.,1.,1.,
1.,1.,1.,1.,1.,1.))
REPRESENTATION_ITEM('')
);
#119=(
BOUNDED_CURVE()
B_SPLINE_CURVE(5,(#31969,#31970,#31971,#31972,#31973,#31974,#31975,#31976,
#31977,#31978,#31979,#31980,#31981,#31982,#31983,#31984,#31985,#31986,#31987,
#31988,#31989,#31990,#31991,#31992,#31993,#31994,#31995,#31996,#31997,#31998,
#31999,#32000,#32001,#32002,#32003,#32004,#32005,#32006,#32007,#32008,#32009,
#32010,#32011,#32012,#32013,#32014,#32015,#32016,#32017,#32018,#32019,#32020,
#32021,#32022,#32023,#32024,#32025,#32026,#32027,#32028,#32029,#32030,#32031,
#32032,#32033,#32034,#32035,#32036,#32037,#32038),.UNSPECIFIED.,.F.,.F.)
B_SPLINE_CURVE_WITH_KNOTS((6,1,1,1,1,1,1,1,1,1,1,1,1,1,1,1,1,1,1,1,1,1,
1,1,1,1,1,1,1,1,1,1,1,1,1,1,1,1,1,1,1,1,1,1,1,1,1,1,1,1,1,1,1,1,1,1,1,1,
1,1,1,1,1,1,1,6),(-1.,-0.984615384615383,-0.969230769230768,-0.953846153846152,
-0.938461538461537,-0.923076923076922,-0.907692307692306,-0.892307692307691,
-0.876923076923076,-0.86153846153846,-0.846153846153845,-0.83076923076923,
-0.815384615384614,-0.799999999999999,-0.784615384615384,-0.769230769230768,
-0.753846153846153,-0.738461538461538,-0.723076923076922,-0.707692307692307,
-0.692307692307692,-0.676923076923076,-0.661538461538461,-0.646153846153846,
-0.63076923076923,-0.615384615384615,-0.6,-0.584615384615384,-0.569230769230769,
-0.553846153846154,-0.538461538461538,-0.523076923076923,-0.507692307692308,
-0.492307692307692,-0.476923076923077,-0.461538461538462,-0.446153846153846,
-0.430769230769231,-0.415384615384615,-0.4,-0.384615384615385,-0.369230769230769,
-0.353846153846154,-0.338461538461538,-0.323076923076923,-0.307692307692308,
-0.292307692307692,-0.276923076923077,-0.261538461538462,-0.246153846153846,
-0.230769230769231,-0.215384615384615,-0.2,-0.184615384615385,-0.169230769230769,
-0.153846153846154,-0.138461538461538,-0.123076923076923,-0.107692307692308,
-0.0923076923076923,-0.0769230769230769,-0.0615384615384615,-0.0461538461538462,
-0.0307692307692308,-0.0153846153846154,0.),.UNSPECIFIED.)
CURVE()
GEOMETRIC_REPRESENTATION_ITEM()
RATIONAL_B_SPLINE_CURVE((1.,1.,1.,1.,1.,1.,1.,1.,1.,1.,1.,1.,1.,1.,1.,1.,
1.,1.,1.,1.,1.,1.,1.,1.,1.,1.,1.,1.,1.,1.,1.,1.,1.,1.,1.,1.,1.,1.,1.,1.,
1.,1.,1.,1.,1.,1.,1.,1.,1.,1.,1.,1.,1.,1.,1.,1.,1.,1.,1.,1.,1.,1.,1.,1.,
1.,1.,1.,1.,1.,1.))
REPRESENTATION_ITEM('')
);
#120=(
BOUNDED_CURVE()
B_SPLINE_CURVE(5,(#32185,#32186,#32187,#32188,#32189,#32190,#32191,#32192,
#32193,#32194,#32195,#32196,#32197,#32198,#32199,#32200,#32201,#32202,#32203,
#32204,#32205,#32206,#32207,#32208,#32209,#32210,#32211,#32212,#32213,#32214,
#32215,#32216,#32217,#32218,#32219,#32220,#32221,#32222,#32223,#32224,#32225,
#32226,#32227,#32228,#32229,#32230,#32231,#32232,#32233,#32234,#32235,#32236,
#32237,#32238,#32239,#32240,#32241,#32242,#32243,#32244,#32245,#32246,#32247,
#32248,#32249,#32250,#32251,#32252,#32253,#32254),.UNSPECIFIED.,.F.,.F.)
B_SPLINE_CURVE_WITH_KNOTS((6,1,1,1,1,1,1,1,1,1,1,1,1,1,1,1,1,1,1,1,1,1,
1,1,1,1,1,1,1,1,1,1,1,1,1,1,1,1,1,1,1,1,1,1,1,1,1,1,1,1,1,1,1,1,1,1,1,1,
1,1,1,1,1,1,1,6),(-1.,-0.984615384615383,-0.969230769230768,-0.953846153846152,
-0.938461538461537,-0.923076923076922,-0.907692307692306,-0.892307692307691,
-0.876923076923076,-0.86153846153846,-0.846153846153845,-0.83076923076923,
-0.815384615384614,-0.799999999999999,-0.784615384615384,-0.769230769230768,
-0.753846153846153,-0.738461538461538,-0.723076923076922,-0.707692307692307,
-0.692307692307692,-0.676923076923076,-0.661538461538461,-0.646153846153846,
-0.63076923076923,-0.615384615384615,-0.6,-0.584615384615384,-0.569230769230769,
-0.553846153846154,-0.538461538461538,-0.523076923076923,-0.507692307692308,
-0.492307692307692,-0.476923076923077,-0.461538461538462,-0.446153846153846,
-0.430769230769231,-0.415384615384615,-0.4,-0.384615384615385,-0.369230769230769,
-0.353846153846154,-0.338461538461538,-0.323076923076923,-0.307692307692308,
-0.292307692307692,-0.276923076923077,-0.261538461538462,-0.246153846153846,
-0.230769230769231,-0.215384615384615,-0.2,-0.184615384615385,-0.169230769230769,
-0.153846153846154,-0.138461538461538,-0.123076923076923,-0.107692307692308,
-0.0923076923076923,-0.0769230769230769,-0.0615384615384615,-0.0461538461538462,
-0.0307692307692308,-0.0153846153846154,0.),.UNSPECIFIED.)
CURVE()
GEOMETRIC_REPRESENTATION_ITEM()
RATIONAL_B_SPLINE_CURVE((1.,1.,1.,1.,1.,1.,1.,1.,1.,1.,1.,1.,1.,1.,1.,1.,
1.,1.,1.,1.,1.,1.,1.,1.,1.,1.,1.,1.,1.,1.,1.,1.,1.,1.,1.,1.,1.,1.,1.,1.,
1.,1.,1.,1.,1.,1.,1.,1.,1.,1.,1.,1.,1.,1.,1.,1.,1.,1.,1.,1.,1.,1.,1.,1.,
1.,1.,1.,1.,1.,1.))
REPRESENTATION_ITEM('')
);
#121=(
BOUNDED_CURVE()
B_SPLINE_CURVE(5,(#32401,#32402,#32403,#32404,#32405,#32406,#32407,#32408,
#32409,#32410,#32411,#32412,#32413,#32414,#32415,#32416,#32417,#32418,#32419,
#32420,#32421,#32422,#32423,#32424,#32425,#32426,#32427,#32428,#32429,#32430,
#32431,#32432,#32433,#32434,#32435,#32436,#32437,#32438,#32439,#32440,#32441,
#32442,#32443,#32444,#32445,#32446,#32447,#32448,#32449,#32450,#32451,#32452,
#32453,#32454,#32455,#32456,#32457,#32458,#32459,#32460,#32461,#32462,#32463,
#32464,#32465,#32466,#32467,#32468,#32469,#32470),.UNSPECIFIED.,.F.,.F.)
B_SPLINE_CURVE_WITH_KNOTS((6,1,1,1,1,1,1,1,1,1,1,1,1,1,1,1,1,1,1,1,1,1,
1,1,1,1,1,1,1,1,1,1,1,1,1,1,1,1,1,1,1,1,1,1,1,1,1,1,1,1,1,1,1,1,1,1,1,1,
1,1,1,1,1,1,1,6),(-1.,-0.984615384615383,-0.969230769230768,-0.953846153846152,
-0.938461538461537,-0.923076923076922,-0.907692307692306,-0.892307692307691,
-0.876923076923076,-0.86153846153846,-0.846153846153845,-0.83076923076923,
-0.815384615384614,-0.799999999999999,-0.784615384615384,-0.769230769230768,
-0.753846153846153,-0.738461538461538,-0.723076923076922,-0.707692307692307,
-0.692307692307692,-0.676923076923076,-0.661538461538461,-0.646153846153846,
-0.63076923076923,-0.615384615384615,-0.6,-0.584615384615384,-0.569230769230769,
-0.553846153846154,-0.538461538461538,-0.523076923076923,-0.507692307692308,
-0.492307692307692,-0.476923076923077,-0.461538461538462,-0.446153846153846,
-0.430769230769231,-0.415384615384615,-0.4,-0.384615384615385,-0.369230769230769,
-0.353846153846154,-0.338461538461538,-0.323076923076923,-0.307692307692308,
-0.292307692307692,-0.276923076923077,-0.261538461538462,-0.246153846153846,
-0.230769230769231,-0.215384615384615,-0.2,-0.184615384615385,-0.169230769230769,
-0.153846153846154,-0.138461538461538,-0.123076923076923,-0.107692307692308,
-0.0923076923076923,-0.0769230769230769,-0.0615384615384615,-0.0461538461538462,
-0.0307692307692308,-0.0153846153846154,0.),.UNSPECIFIED.)
CURVE()
GEOMETRIC_REPRESENTATION_ITEM()
RATIONAL_B_SPLINE_CURVE((1.,1.,1.,1.,1.,1.,1.,1.,1.,1.,1.,1.,1.,1.,1.,1.,
1.,1.,1.,1.,1.,1.,1.,1.,1.,1.,1.,1.,1.,1.,1.,1.,1.,1.,1.,1.,1.,1.,1.,1.,
1.,1.,1.,1.,1.,1.,1.,1.,1.,1.,1.,1.,1.,1.,1.,1.,1.,1.,1.,1.,1.,1.,1.,1.,
1.,1.,1.,1.,1.,1.))
REPRESENTATION_ITEM('')
);
#122=(
BOUNDED_CURVE()
B_SPLINE_CURVE(5,(#32617,#32618,#32619,#32620,#32621,#32622,#32623,#32624,
#32625,#32626,#32627,#32628,#32629,#32630,#32631,#32632,#32633,#32634,#32635,
#32636,#32637,#32638,#32639,#32640,#32641,#32642,#32643,#32644,#32645,#32646,
#32647,#32648,#32649,#32650,#32651,#32652,#32653,#32654,#32655,#32656,#32657,
#32658,#32659,#32660,#32661,#32662,#32663,#32664,#32665,#32666,#32667,#32668,
#32669,#32670,#32671,#32672,#32673,#32674,#32675,#32676,#32677,#32678,#32679,
#32680,#32681,#32682,#32683,#32684,#32685,#32686),.UNSPECIFIED.,.F.,.F.)
B_SPLINE_CURVE_WITH_KNOTS((6,1,1,1,1,1,1,1,1,1,1,1,1,1,1,1,1,1,1,1,1,1,
1,1,1,1,1,1,1,1,1,1,1,1,1,1,1,1,1,1,1,1,1,1,1,1,1,1,1,1,1,1,1,1,1,1,1,1,
1,1,1,1,1,1,1,6),(-1.,-0.984615384615383,-0.969230769230768,-0.953846153846152,
-0.938461538461537,-0.923076923076922,-0.907692307692306,-0.892307692307691,
-0.876923076923076,-0.86153846153846,-0.846153846153845,-0.83076923076923,
-0.815384615384614,-0.799999999999999,-0.784615384615384,-0.769230769230768,
-0.753846153846153,-0.738461538461538,-0.723076923076922,-0.707692307692307,
-0.692307692307692,-0.676923076923076,-0.661538461538461,-0.646153846153846,
-0.63076923076923,-0.615384615384615,-0.6,-0.584615384615384,-0.569230769230769,
-0.553846153846154,-0.538461538461538,-0.523076923076923,-0.507692307692308,
-0.492307692307692,-0.476923076923077,-0.461538461538462,-0.446153846153846,
-0.430769230769231,-0.415384615384615,-0.4,-0.384615384615385,-0.369230769230769,
-0.353846153846154,-0.338461538461538,-0.323076923076923,-0.307692307692308,
-0.292307692307692,-0.276923076923077,-0.261538461538462,-0.246153846153846,
-0.230769230769231,-0.215384615384615,-0.2,-0.184615384615385,-0.169230769230769,
-0.153846153846154,-0.138461538461538,-0.123076923076923,-0.107692307692308,
-0.0923076923076923,-0.0769230769230769,-0.0615384615384615,-0.0461538461538462,
-0.0307692307692308,-0.0153846153846154,0.),.UNSPECIFIED.)
CURVE()
GEOMETRIC_REPRESENTATION_ITEM()
RATIONAL_B_SPLINE_CURVE((1.,1.,1.,1.,1.,1.,1.,1.,1.,1.,1.,1.,1.,1.,1.,1.,
1.,1.,1.,1.,1.,1.,1.,1.,1.,1.,1.,1.,1.,1.,1.,1.,1.,1.,1.,1.,1.,1.,1.,1.,
1.,1.,1.,1.,1.,1.,1.,1.,1.,1.,1.,1.,1.,1.,1.,1.,1.,1.,1.,1.,1.,1.,1.,1.,
1.,1.,1.,1.,1.,1.))
REPRESENTATION_ITEM('')
);
#123=(
BOUNDED_CURVE()
B_SPLINE_CURVE(5,(#32833,#32834,#32835,#32836,#32837,#32838,#32839,#32840,
#32841,#32842,#32843,#32844,#32845,#32846,#32847,#32848,#32849,#32850,#32851,
#32852,#32853,#32854,#32855,#32856,#32857,#32858,#32859,#32860,#32861,#32862,
#32863,#32864,#32865,#32866,#32867,#32868,#32869,#32870,#32871,#32872,#32873,
#32874,#32875,#32876,#32877,#32878,#32879,#32880,#32881,#32882,#32883,#32884,
#32885,#32886,#32887,#32888,#32889,#32890,#32891,#32892,#32893,#32894,#32895,
#32896,#32897,#32898,#32899,#32900,#32901,#32902),.UNSPECIFIED.,.F.,.F.)
B_SPLINE_CURVE_WITH_KNOTS((6,1,1,1,1,1,1,1,1,1,1,1,1,1,1,1,1,1,1,1,1,1,
1,1,1,1,1,1,1,1,1,1,1,1,1,1,1,1,1,1,1,1,1,1,1,1,1,1,1,1,1,1,1,1,1,1,1,1,
1,1,1,1,1,1,1,6),(-1.,-0.984615384615383,-0.969230769230768,-0.953846153846152,
-0.938461538461537,-0.923076923076922,-0.907692307692306,-0.892307692307691,
-0.876923076923076,-0.86153846153846,-0.846153846153845,-0.83076923076923,
-0.815384615384614,-0.799999999999999,-0.784615384615384,-0.769230769230768,
-0.753846153846153,-0.738461538461538,-0.723076923076922,-0.707692307692307,
-0.692307692307692,-0.676923076923076,-0.661538461538461,-0.646153846153846,
-0.63076923076923,-0.615384615384615,-0.6,-0.584615384615384,-0.569230769230769,
-0.553846153846154,-0.538461538461538,-0.523076923076923,-0.507692307692308,
-0.492307692307692,-0.476923076923077,-0.461538461538462,-0.446153846153846,
-0.430769230769231,-0.415384615384615,-0.4,-0.384615384615385,-0.369230769230769,
-0.353846153846154,-0.338461538461538,-0.323076923076923,-0.307692307692308,
-0.292307692307692,-0.276923076923077,-0.261538461538462,-0.246153846153846,
-0.230769230769231,-0.215384615384615,-0.2,-0.184615384615385,-0.169230769230769,
-0.153846153846154,-0.138461538461538,-0.123076923076923,-0.107692307692308,
-0.0923076923076923,-0.0769230769230769,-0.0615384615384615,-0.0461538461538462,
-0.0307692307692308,-0.0153846153846154,0.),.UNSPECIFIED.)
CURVE()
GEOMETRIC_REPRESENTATION_ITEM()
RATIONAL_B_SPLINE_CURVE((1.,1.,1.,1.,1.,1.,1.,1.,1.,1.,1.,1.,1.,1.,1.,1.,
1.,1.,1.,1.,1.,1.,1.,1.,1.,1.,1.,1.,1.,1.,1.,1.,1.,1.,1.,1.,1.,1.,1.,1.,
1.,1.,1.,1.,1.,1.,1.,1.,1.,1.,1.,1.,1.,1.,1.,1.,1.,1.,1.,1.,1.,1.,1.,1.,
1.,1.,1.,1.,1.,1.))
REPRESENTATION_ITEM('')
);
#124=(
BOUNDED_CURVE()
B_SPLINE_CURVE(5,(#33049,#33050,#33051,#33052,#33053,#33054,#33055,#33056,
#33057,#33058,#33059,#33060,#33061,#33062,#33063,#33064,#33065,#33066,#33067,
#33068,#33069,#33070,#33071,#33072,#33073,#33074,#33075,#33076,#33077,#33078,
#33079,#33080,#33081,#33082,#33083,#33084,#33085,#33086,#33087,#33088,#33089,
#33090,#33091,#33092,#33093,#33094,#33095,#33096,#33097,#33098,#33099,#33100,
#33101,#33102,#33103,#33104,#33105,#33106,#33107,#33108,#33109,#33110,#33111,
#33112,#33113,#33114,#33115,#33116,#33117,#33118),.UNSPECIFIED.,.F.,.F.)
B_SPLINE_CURVE_WITH_KNOTS((6,1,1,1,1,1,1,1,1,1,1,1,1,1,1,1,1,1,1,1,1,1,
1,1,1,1,1,1,1,1,1,1,1,1,1,1,1,1,1,1,1,1,1,1,1,1,1,1,1,1,1,1,1,1,1,1,1,1,
1,1,1,1,1,1,1,6),(-1.,-0.984615384615383,-0.969230769230768,-0.953846153846152,
-0.938461538461537,-0.923076923076922,-0.907692307692306,-0.892307692307691,
-0.876923076923076,-0.86153846153846,-0.846153846153845,-0.83076923076923,
-0.815384615384614,-0.799999999999999,-0.784615384615384,-0.769230769230768,
-0.753846153846153,-0.738461538461538,-0.723076923076922,-0.707692307692307,
-0.692307692307692,-0.676923076923076,-0.661538461538461,-0.646153846153846,
-0.63076923076923,-0.615384615384615,-0.6,-0.584615384615384,-0.569230769230769,
-0.553846153846154,-0.538461538461538,-0.523076923076923,-0.507692307692308,
-0.492307692307692,-0.476923076923077,-0.461538461538462,-0.446153846153846,
-0.430769230769231,-0.415384615384615,-0.4,-0.384615384615385,-0.369230769230769,
-0.353846153846154,-0.338461538461538,-0.323076923076923,-0.307692307692308,
-0.292307692307692,-0.276923076923077,-0.261538461538462,-0.246153846153846,
-0.230769230769231,-0.215384615384615,-0.2,-0.184615384615385,-0.169230769230769,
-0.153846153846154,-0.138461538461538,-0.123076923076923,-0.107692307692308,
-0.0923076923076923,-0.0769230769230769,-0.0615384615384615,-0.0461538461538462,
-0.0307692307692308,-0.0153846153846154,0.),.UNSPECIFIED.)
CURVE()
GEOMETRIC_REPRESENTATION_ITEM()
RATIONAL_B_SPLINE_CURVE((1.,1.,1.,1.,1.,1.,1.,1.,1.,1.,1.,1.,1.,1.,1.,1.,
1.,1.,1.,1.,1.,1.,1.,1.,1.,1.,1.,1.,1.,1.,1.,1.,1.,1.,1.,1.,1.,1.,1.,1.,
1.,1.,1.,1.,1.,1.,1.,1.,1.,1.,1.,1.,1.,1.,1.,1.,1.,1.,1.,1.,1.,1.,1.,1.,
1.,1.,1.,1.,1.,1.))
REPRESENTATION_ITEM('')
);
#125=(
BOUNDED_CURVE()
B_SPLINE_CURVE(5,(#33265,#33266,#33267,#33268,#33269,#33270,#33271,#33272,
#33273,#33274,#33275,#33276,#33277,#33278,#33279,#33280,#33281,#33282,#33283,
#33284,#33285,#33286,#33287,#33288,#33289,#33290,#33291,#33292,#33293,#33294,
#33295,#33296,#33297,#33298,#33299,#33300,#33301,#33302,#33303,#33304,#33305,
#33306,#33307,#33308,#33309,#33310,#33311,#33312,#33313,#33314,#33315,#33316,
#33317,#33318,#33319,#33320,#33321,#33322,#33323,#33324,#33325,#33326,#33327,
#33328,#33329,#33330,#33331,#33332,#33333,#33334),.UNSPECIFIED.,.F.,.F.)
B_SPLINE_CURVE_WITH_KNOTS((6,1,1,1,1,1,1,1,1,1,1,1,1,1,1,1,1,1,1,1,1,1,
1,1,1,1,1,1,1,1,1,1,1,1,1,1,1,1,1,1,1,1,1,1,1,1,1,1,1,1,1,1,1,1,1,1,1,1,
1,1,1,1,1,1,1,6),(-1.,-0.984615384615383,-0.969230769230768,-0.953846153846152,
-0.938461538461537,-0.923076923076922,-0.907692307692306,-0.892307692307691,
-0.876923076923076,-0.86153846153846,-0.846153846153845,-0.83076923076923,
-0.815384615384614,-0.799999999999999,-0.784615384615384,-0.769230769230768,
-0.753846153846153,-0.738461538461538,-0.723076923076922,-0.707692307692307,
-0.692307692307692,-0.676923076923076,-0.661538461538461,-0.646153846153846,
-0.63076923076923,-0.615384615384615,-0.6,-0.584615384615384,-0.569230769230769,
-0.553846153846154,-0.538461538461538,-0.523076923076923,-0.507692307692308,
-0.492307692307692,-0.476923076923077,-0.461538461538462,-0.446153846153846,
-0.430769230769231,-0.415384615384615,-0.4,-0.384615384615385,-0.369230769230769,
-0.353846153846154,-0.338461538461538,-0.323076923076923,-0.307692307692308,
-0.292307692307692,-0.276923076923077,-0.261538461538462,-0.246153846153846,
-0.230769230769231,-0.215384615384615,-0.2,-0.184615384615385,-0.169230769230769,
-0.153846153846154,-0.138461538461538,-0.123076923076923,-0.107692307692308,
-0.0923076923076923,-0.0769230769230769,-0.0615384615384615,-0.0461538461538462,
-0.0307692307692308,-0.0153846153846154,0.),.UNSPECIFIED.)
CURVE()
GEOMETRIC_REPRESENTATION_ITEM()
RATIONAL_B_SPLINE_CURVE((1.,1.,1.,1.,1.,1.,1.,1.,1.,1.,1.,1.,1.,1.,1.,1.,
1.,1.,1.,1.,1.,1.,1.,1.,1.,1.,1.,1.,1.,1.,1.,1.,1.,1.,1.,1.,1.,1.,1.,1.,
1.,1.,1.,1.,1.,1.,1.,1.,1.,1.,1.,1.,1.,1.,1.,1.,1.,1.,1.,1.,1.,1.,1.,1.,
1.,1.,1.,1.,1.,1.))
REPRESENTATION_ITEM('')
);
#126=(
BOUNDED_CURVE()
B_SPLINE_CURVE(5,(#33481,#33482,#33483,#33484,#33485,#33486,#33487,#33488,
#33489,#33490,#33491,#33492,#33493,#33494,#33495,#33496,#33497,#33498,#33499,
#33500,#33501,#33502,#33503,#33504,#33505,#33506,#33507,#33508,#33509,#33510,
#33511,#33512,#33513,#33514,#33515,#33516,#33517,#33518,#33519,#33520,#33521,
#33522,#33523,#33524,#33525,#33526,#33527,#33528,#33529,#33530,#33531,#33532,
#33533,#33534,#33535,#33536,#33537,#33538,#33539,#33540,#33541,#33542,#33543,
#33544,#33545,#33546,#33547,#33548,#33549,#33550),.UNSPECIFIED.,.F.,.F.)
B_SPLINE_CURVE_WITH_KNOTS((6,1,1,1,1,1,1,1,1,1,1,1,1,1,1,1,1,1,1,1,1,1,
1,1,1,1,1,1,1,1,1,1,1,1,1,1,1,1,1,1,1,1,1,1,1,1,1,1,1,1,1,1,1,1,1,1,1,1,
1,1,1,1,1,1,1,6),(-1.,-0.984615384615383,-0.969230769230768,-0.953846153846152,
-0.938461538461537,-0.923076923076922,-0.907692307692306,-0.892307692307691,
-0.876923076923076,-0.86153846153846,-0.846153846153845,-0.83076923076923,
-0.815384615384614,-0.799999999999999,-0.784615384615384,-0.769230769230768,
-0.753846153846153,-0.738461538461538,-0.723076923076922,-0.707692307692307,
-0.692307692307692,-0.676923076923076,-0.661538461538461,-0.646153846153846,
-0.63076923076923,-0.615384615384615,-0.6,-0.584615384615384,-0.569230769230769,
-0.553846153846154,-0.538461538461538,-0.523076923076923,-0.507692307692308,
-0.492307692307692,-0.476923076923077,-0.461538461538462,-0.446153846153846,
-0.430769230769231,-0.415384615384615,-0.4,-0.384615384615385,-0.369230769230769,
-0.353846153846154,-0.338461538461538,-0.323076923076923,-0.307692307692308,
-0.292307692307692,-0.276923076923077,-0.261538461538462,-0.246153846153846,
-0.230769230769231,-0.215384615384615,-0.2,-0.184615384615385,-0.169230769230769,
-0.153846153846154,-0.138461538461538,-0.123076923076923,-0.107692307692308,
-0.0923076923076923,-0.0769230769230769,-0.0615384615384615,-0.0461538461538462,
-0.0307692307692308,-0.0153846153846154,0.),.UNSPECIFIED.)
CURVE()
GEOMETRIC_REPRESENTATION_ITEM()
RATIONAL_B_SPLINE_CURVE((1.,1.,1.,1.,1.,1.,1.,1.,1.,1.,1.,1.,1.,1.,1.,1.,
1.,1.,1.,1.,1.,1.,1.,1.,1.,1.,1.,1.,1.,1.,1.,1.,1.,1.,1.,1.,1.,1.,1.,1.,
1.,1.,1.,1.,1.,1.,1.,1.,1.,1.,1.,1.,1.,1.,1.,1.,1.,1.,1.,1.,1.,1.,1.,1.,
1.,1.,1.,1.,1.,1.))
REPRESENTATION_ITEM('')
);
#127=(
BOUNDED_CURVE()
B_SPLINE_CURVE(5,(#33697,#33698,#33699,#33700,#33701,#33702,#33703,#33704,
#33705,#33706,#33707,#33708,#33709,#33710,#33711,#33712,#33713,#33714,#33715,
#33716,#33717,#33718,#33719,#33720,#33721,#33722,#33723,#33724,#33725,#33726,
#33727,#33728,#33729,#33730,#33731,#33732,#33733,#33734,#33735,#33736,#33737,
#33738,#33739,#33740,#33741,#33742,#33743,#33744,#33745,#33746,#33747,#33748,
#33749,#33750,#33751,#33752,#33753,#33754,#33755,#33756,#33757,#33758,#33759,
#33760,#33761,#33762,#33763,#33764,#33765,#33766),.UNSPECIFIED.,.F.,.F.)
B_SPLINE_CURVE_WITH_KNOTS((6,1,1,1,1,1,1,1,1,1,1,1,1,1,1,1,1,1,1,1,1,1,
1,1,1,1,1,1,1,1,1,1,1,1,1,1,1,1,1,1,1,1,1,1,1,1,1,1,1,1,1,1,1,1,1,1,1,1,
1,1,1,1,1,1,1,6),(-1.,-0.984615384615383,-0.969230769230768,-0.953846153846152,
-0.938461538461537,-0.923076923076922,-0.907692307692306,-0.892307692307691,
-0.876923076923076,-0.86153846153846,-0.846153846153845,-0.83076923076923,
-0.815384615384614,-0.799999999999999,-0.784615384615384,-0.769230769230768,
-0.753846153846153,-0.738461538461538,-0.723076923076922,-0.707692307692307,
-0.692307692307692,-0.676923076923076,-0.661538461538461,-0.646153846153846,
-0.63076923076923,-0.615384615384615,-0.6,-0.584615384615384,-0.569230769230769,
-0.553846153846154,-0.538461538461538,-0.523076923076923,-0.507692307692308,
-0.492307692307692,-0.476923076923077,-0.461538461538462,-0.446153846153846,
-0.430769230769231,-0.415384615384615,-0.4,-0.384615384615385,-0.369230769230769,
-0.353846153846154,-0.338461538461538,-0.323076923076923,-0.307692307692308,
-0.292307692307692,-0.276923076923077,-0.261538461538462,-0.246153846153846,
-0.230769230769231,-0.215384615384615,-0.2,-0.184615384615385,-0.169230769230769,
-0.153846153846154,-0.138461538461538,-0.123076923076923,-0.107692307692308,
-0.0923076923076923,-0.0769230769230769,-0.0615384615384615,-0.0461538461538462,
-0.0307692307692308,-0.0153846153846154,0.),.UNSPECIFIED.)
CURVE()
GEOMETRIC_REPRESENTATION_ITEM()
RATIONAL_B_SPLINE_CURVE((1.,1.,1.,1.,1.,1.,1.,1.,1.,1.,1.,1.,1.,1.,1.,1.,
1.,1.,1.,1.,1.,1.,1.,1.,1.,1.,1.,1.,1.,1.,1.,1.,1.,1.,1.,1.,1.,1.,1.,1.,
1.,1.,1.,1.,1.,1.,1.,1.,1.,1.,1.,1.,1.,1.,1.,1.,1.,1.,1.,1.,1.,1.,1.,1.,
1.,1.,1.,1.,1.,1.))
REPRESENTATION_ITEM('')
);
#128=(
BOUNDED_CURVE()
B_SPLINE_CURVE(5,(#33913,#33914,#33915,#33916,#33917,#33918,#33919,#33920,
#33921,#33922,#33923,#33924,#33925,#33926,#33927,#33928,#33929,#33930,#33931,
#33932,#33933,#33934,#33935,#33936,#33937,#33938,#33939,#33940,#33941,#33942,
#33943,#33944,#33945,#33946,#33947,#33948,#33949,#33950,#33951,#33952,#33953,
#33954,#33955,#33956,#33957,#33958,#33959,#33960,#33961,#33962,#33963,#33964,
#33965,#33966,#33967,#33968,#33969,#33970,#33971,#33972,#33973,#33974,#33975,
#33976,#33977,#33978,#33979,#33980,#33981,#33982),.UNSPECIFIED.,.F.,.F.)
B_SPLINE_CURVE_WITH_KNOTS((6,1,1,1,1,1,1,1,1,1,1,1,1,1,1,1,1,1,1,1,1,1,
1,1,1,1,1,1,1,1,1,1,1,1,1,1,1,1,1,1,1,1,1,1,1,1,1,1,1,1,1,1,1,1,1,1,1,1,
1,1,1,1,1,1,1,6),(-1.,-0.984615384615383,-0.969230769230768,-0.953846153846152,
-0.938461538461537,-0.923076923076922,-0.907692307692306,-0.892307692307691,
-0.876923076923076,-0.86153846153846,-0.846153846153845,-0.83076923076923,
-0.815384615384614,-0.799999999999999,-0.784615384615384,-0.769230769230768,
-0.753846153846153,-0.738461538461538,-0.723076923076922,-0.707692307692307,
-0.692307692307692,-0.676923076923076,-0.661538461538461,-0.646153846153846,
-0.63076923076923,-0.615384615384615,-0.6,-0.584615384615384,-0.569230769230769,
-0.553846153846154,-0.538461538461538,-0.523076923076923,-0.507692307692308,
-0.492307692307692,-0.476923076923077,-0.461538461538462,-0.446153846153846,
-0.430769230769231,-0.415384615384615,-0.4,-0.384615384615385,-0.369230769230769,
-0.353846153846154,-0.338461538461538,-0.323076923076923,-0.307692307692308,
-0.292307692307692,-0.276923076923077,-0.261538461538462,-0.246153846153846,
-0.230769230769231,-0.215384615384615,-0.2,-0.184615384615385,-0.169230769230769,
-0.153846153846154,-0.138461538461538,-0.123076923076923,-0.107692307692308,
-0.0923076923076923,-0.0769230769230769,-0.0615384615384615,-0.0461538461538462,
-0.0307692307692308,-0.0153846153846154,0.),.UNSPECIFIED.)
CURVE()
GEOMETRIC_REPRESENTATION_ITEM()
RATIONAL_B_SPLINE_CURVE((1.,1.,1.,1.,1.,1.,1.,1.,1.,1.,1.,1.,1.,1.,1.,1.,
1.,1.,1.,1.,1.,1.,1.,1.,1.,1.,1.,1.,1.,1.,1.,1.,1.,1.,1.,1.,1.,1.,1.,1.,
1.,1.,1.,1.,1.,1.,1.,1.,1.,1.,1.,1.,1.,1.,1.,1.,1.,1.,1.,1.,1.,1.,1.,1.,
1.,1.,1.,1.,1.,1.))
REPRESENTATION_ITEM('')
);
#129=(
BOUNDED_CURVE()
B_SPLINE_CURVE(5,(#34129,#34130,#34131,#34132,#34133,#34134,#34135,#34136,
#34137,#34138,#34139,#34140,#34141,#34142,#34143,#34144,#34145,#34146,#34147,
#34148,#34149,#34150,#34151,#34152,#34153,#34154,#34155,#34156,#34157,#34158,
#34159,#34160,#34161,#34162,#34163,#34164,#34165,#34166,#34167,#34168,#34169,
#34170,#34171,#34172,#34173,#34174,#34175,#34176,#34177,#34178,#34179,#34180,
#34181,#34182,#34183,#34184,#34185,#34186,#34187,#34188,#34189,#34190,#34191,
#34192,#34193,#34194,#34195,#34196,#34197,#34198),.UNSPECIFIED.,.F.,.F.)
B_SPLINE_CURVE_WITH_KNOTS((6,1,1,1,1,1,1,1,1,1,1,1,1,1,1,1,1,1,1,1,1,1,
1,1,1,1,1,1,1,1,1,1,1,1,1,1,1,1,1,1,1,1,1,1,1,1,1,1,1,1,1,1,1,1,1,1,1,1,
1,1,1,1,1,1,1,6),(-1.,-0.984615384615383,-0.969230769230768,-0.953846153846152,
-0.938461538461537,-0.923076923076922,-0.907692307692306,-0.892307692307691,
-0.876923076923076,-0.86153846153846,-0.846153846153845,-0.83076923076923,
-0.815384615384614,-0.799999999999999,-0.784615384615384,-0.769230769230768,
-0.753846153846153,-0.738461538461538,-0.723076923076922,-0.707692307692307,
-0.692307692307692,-0.676923076923076,-0.661538461538461,-0.646153846153846,
-0.63076923076923,-0.615384615384615,-0.6,-0.584615384615384,-0.569230769230769,
-0.553846153846154,-0.538461538461538,-0.523076923076923,-0.507692307692308,
-0.492307692307692,-0.476923076923077,-0.461538461538462,-0.446153846153846,
-0.430769230769231,-0.415384615384615,-0.4,-0.384615384615385,-0.369230769230769,
-0.353846153846154,-0.338461538461538,-0.323076923076923,-0.307692307692308,
-0.292307692307692,-0.276923076923077,-0.261538461538462,-0.246153846153846,
-0.230769230769231,-0.215384615384615,-0.2,-0.184615384615385,-0.169230769230769,
-0.153846153846154,-0.138461538461538,-0.123076923076923,-0.107692307692308,
-0.0923076923076923,-0.0769230769230769,-0.0615384615384615,-0.0461538461538462,
-0.0307692307692308,-0.0153846153846154,0.),.UNSPECIFIED.)
CURVE()
GEOMETRIC_REPRESENTATION_ITEM()
RATIONAL_B_SPLINE_CURVE((1.,1.,1.,1.,1.,1.,1.,1.,1.,1.,1.,1.,1.,1.,1.,1.,
1.,1.,1.,1.,1.,1.,1.,1.,1.,1.,1.,1.,1.,1.,1.,1.,1.,1.,1.,1.,1.,1.,1.,1.,
1.,1.,1.,1.,1.,1.,1.,1.,1.,1.,1.,1.,1.,1.,1.,1.,1.,1.,1.,1.,1.,1.,1.,1.,
1.,1.,1.,1.,1.,1.))
REPRESENTATION_ITEM('')
);
#130=(
BOUNDED_CURVE()
B_SPLINE_CURVE(5,(#34345,#34346,#34347,#34348,#34349,#34350,#34351,#34352,
#34353,#34354,#34355,#34356,#34357,#34358,#34359,#34360,#34361,#34362,#34363,
#34364,#34365,#34366,#34367,#34368,#34369,#34370,#34371,#34372,#34373,#34374,
#34375,#34376,#34377,#34378,#34379,#34380,#34381,#34382,#34383,#34384,#34385,
#34386,#34387,#34388,#34389,#34390,#34391,#34392,#34393,#34394,#34395,#34396,
#34397,#34398,#34399,#34400,#34401,#34402,#34403,#34404,#34405,#34406,#34407,
#34408,#34409,#34410,#34411,#34412,#34413,#34414),.UNSPECIFIED.,.F.,.F.)
B_SPLINE_CURVE_WITH_KNOTS((6,1,1,1,1,1,1,1,1,1,1,1,1,1,1,1,1,1,1,1,1,1,
1,1,1,1,1,1,1,1,1,1,1,1,1,1,1,1,1,1,1,1,1,1,1,1,1,1,1,1,1,1,1,1,1,1,1,1,
1,1,1,1,1,1,1,6),(-1.,-0.984615384615383,-0.969230769230768,-0.953846153846152,
-0.938461538461537,-0.923076923076922,-0.907692307692306,-0.892307692307691,
-0.876923076923076,-0.86153846153846,-0.846153846153845,-0.83076923076923,
-0.815384615384614,-0.799999999999999,-0.784615384615384,-0.769230769230768,
-0.753846153846153,-0.738461538461538,-0.723076923076922,-0.707692307692307,
-0.692307692307692,-0.676923076923076,-0.661538461538461,-0.646153846153846,
-0.63076923076923,-0.615384615384615,-0.6,-0.584615384615384,-0.569230769230769,
-0.553846153846154,-0.538461538461538,-0.523076923076923,-0.507692307692308,
-0.492307692307692,-0.476923076923077,-0.461538461538462,-0.446153846153846,
-0.430769230769231,-0.415384615384615,-0.4,-0.384615384615385,-0.369230769230769,
-0.353846153846154,-0.338461538461538,-0.323076923076923,-0.307692307692308,
-0.292307692307692,-0.276923076923077,-0.261538461538462,-0.246153846153846,
-0.230769230769231,-0.215384615384615,-0.2,-0.184615384615385,-0.169230769230769,
-0.153846153846154,-0.138461538461538,-0.123076923076923,-0.107692307692308,
-0.0923076923076923,-0.0769230769230769,-0.0615384615384615,-0.0461538461538462,
-0.0307692307692308,-0.0153846153846154,0.),.UNSPECIFIED.)
CURVE()
GEOMETRIC_REPRESENTATION_ITEM()
RATIONAL_B_SPLINE_CURVE((1.,1.,1.,1.,1.,1.,1.,1.,1.,1.,1.,1.,1.,1.,1.,1.,
1.,1.,1.,1.,1.,1.,1.,1.,1.,1.,1.,1.,1.,1.,1.,1.,1.,1.,1.,1.,1.,1.,1.,1.,
1.,1.,1.,1.,1.,1.,1.,1.,1.,1.,1.,1.,1.,1.,1.,1.,1.,1.,1.,1.,1.,1.,1.,1.,
1.,1.,1.,1.,1.,1.))
REPRESENTATION_ITEM('')
);
#131=ITEM_DEFINED_TRANSFORMATION($,$,#14779,#14901);
#132=ITEM_DEFINED_TRANSFORMATION($,$,#14799,#14902);
#133=ITEM_DEFINED_TRANSFORMATION($,$,#14819,#14903);
#134=ITEM_DEFINED_TRANSFORMATION($,$,#14834,#14904);
#135=ITEM_DEFINED_TRANSFORMATION($,$,#14884,#14905);
#136=ITEM_DEFINED_TRANSFORMATION($,$,#15110,#15171);
#137=ITEM_DEFINED_TRANSFORMATION($,$,#15149,#15172);
#138=ITEM_DEFINED_TRANSFORMATION($,$,#15160,#15173);
#139=ITEM_DEFINED_TRANSFORMATION($,$,#14319,#15441);
#140=ITEM_DEFINED_TRANSFORMATION($,$,#14338,#15442);
#141=ITEM_DEFINED_TRANSFORMATION($,$,#14345,#15443);
#142=ITEM_DEFINED_TRANSFORMATION($,$,#14352,#15444);
#143=ITEM_DEFINED_TRANSFORMATION($,$,#14407,#15445);
#144=ITEM_DEFINED_TRANSFORMATION($,$,#14428,#15446);
#145=ITEM_DEFINED_TRANSFORMATION($,$,#14435,#15447);
#146=ITEM_DEFINED_TRANSFORMATION($,$,#14456,#15448);
#147=ITEM_DEFINED_TRANSFORMATION($,$,#14463,#15449);
#148=ITEM_DEFINED_TRANSFORMATION($,$,#14495,#15450);
#149=ITEM_DEFINED_TRANSFORMATION($,$,#14520,#15451);
#150=ITEM_DEFINED_TRANSFORMATION($,$,#14545,#15452);
#151=ITEM_DEFINED_TRANSFORMATION($,$,#14577,#15453);
#152=ITEM_DEFINED_TRANSFORMATION($,$,#14602,#15454);
#153=ITEM_DEFINED_TRANSFORMATION($,$,#14627,#15455);
#154=ITEM_DEFINED_TRANSFORMATION($,$,#14627,#15456);
#155=ITEM_DEFINED_TRANSFORMATION($,$,#14677,#15457);
#156=ITEM_DEFINED_TRANSFORMATION($,$,#14698,#15458);
#157=ITEM_DEFINED_TRANSFORMATION($,$,#15174,#15459);
#158=ITEM_DEFINED_TRANSFORMATION($,$,#14677,#15460);
#159=ITEM_DEFINED_TRANSFORMATION($,$,#14698,#15461);
#160=ITEM_DEFINED_TRANSFORMATION($,$,#15174,#15462);
#161=ITEM_DEFINED_TRANSFORMATION($,$,#14677,#15463);
#162=ITEM_DEFINED_TRANSFORMATION($,$,#14698,#15464);
#163=ITEM_DEFINED_TRANSFORMATION($,$,#15174,#15465);
#164=ITEM_DEFINED_TRANSFORMATION($,$,#14677,#15466);
#165=ITEM_DEFINED_TRANSFORMATION($,$,#14698,#15467);
#166=ITEM_DEFINED_TRANSFORMATION($,$,#15174,#15468);
#167=ITEM_DEFINED_TRANSFORMATION($,$,#14677,#15469);
#168=ITEM_DEFINED_TRANSFORMATION($,$,#14698,#15470);
#169=ITEM_DEFINED_TRANSFORMATION($,$,#15174,#15471);
#170=ITEM_DEFINED_TRANSFORMATION($,$,#14677,#15472);
#171=ITEM_DEFINED_TRANSFORMATION($,$,#14698,#15473);
#172=ITEM_DEFINED_TRANSFORMATION($,$,#15174,#15474);
#173=ITEM_DEFINED_TRANSFORMATION($,$,#14677,#15475);
#174=ITEM_DEFINED_TRANSFORMATION($,$,#14698,#15476);
#175=ITEM_DEFINED_TRANSFORMATION($,$,#15174,#15477);
#176=ITEM_DEFINED_TRANSFORMATION($,$,#14677,#15478);
#177=ITEM_DEFINED_TRANSFORMATION($,$,#14698,#15479);
#178=ITEM_DEFINED_TRANSFORMATION($,$,#15174,#15480);
#179=ITEM_DEFINED_TRANSFORMATION($,$,#14709,#15481);
#180=ITEM_DEFINED_TRANSFORMATION($,$,#15415,#15482);
#181=ITEM_DEFINED_TRANSFORMATION($,$,#15415,#15483);
#182=ITEM_DEFINED_TRANSFORMATION($,$,#15415,#15484);
#183=ITEM_DEFINED_TRANSFORMATION($,$,#15415,#15485);
#184=ITEM_DEFINED_TRANSFORMATION($,$,#14752,#15486);
#185=ITEM_DEFINED_TRANSFORMATION($,$,#14752,#15487);
#186=ITEM_DEFINED_TRANSFORMATION($,$,#14752,#15488);
#187=ITEM_DEFINED_TRANSFORMATION($,$,#14752,#15489);
#188=ITEM_DEFINED_TRANSFORMATION($,$,#15415,#15490);
#189=ITEM_DEFINED_TRANSFORMATION($,$,#15415,#15491);
#190=ITEM_DEFINED_TRANSFORMATION($,$,#14778,#15492);
#191=ITEM_DEFINED_TRANSFORMATION($,$,#14906,#15493);
#192=ITEM_DEFINED_TRANSFORMATION($,$,#14906,#15494);
#193=ITEM_DEFINED_TRANSFORMATION($,$,#14906,#15495);
#194=ITEM_DEFINED_TRANSFORMATION($,$,#14906,#15496);
#195=ITEM_DEFINED_TRANSFORMATION($,$,#14906,#15497);
#196=ITEM_DEFINED_TRANSFORMATION($,$,#14906,#15498);
#197=ITEM_DEFINED_TRANSFORMATION($,$,#14906,#15499);
#198=ITEM_DEFINED_TRANSFORMATION($,$,#14906,#15500);
#199=ITEM_DEFINED_TRANSFORMATION($,$,#15415,#15501);
#200=ITEM_DEFINED_TRANSFORMATION($,$,#15415,#15502);
#201=ITEM_DEFINED_TRANSFORMATION($,$,#14778,#15503);
#202=ITEM_DEFINED_TRANSFORMATION($,$,#14906,#15504);
#203=ITEM_DEFINED_TRANSFORMATION($,$,#14906,#15505);
#204=ITEM_DEFINED_TRANSFORMATION($,$,#14906,#15506);
#205=ITEM_DEFINED_TRANSFORMATION($,$,#14906,#15507);
#206=ITEM_DEFINED_TRANSFORMATION($,$,#14906,#15508);
#207=ITEM_DEFINED_TRANSFORMATION($,$,#14906,#15509);
#208=ITEM_DEFINED_TRANSFORMATION($,$,#14906,#15510);
#209=ITEM_DEFINED_TRANSFORMATION($,$,#14906,#15511);
#210=ITEM_DEFINED_TRANSFORMATION($,$,#14931,#15512);
#211=ITEM_DEFINED_TRANSFORMATION($,$,#14962,#15513);
#212=ITEM_DEFINED_TRANSFORMATION($,$,#15109,#15514);
#213=ITEM_DEFINED_TRANSFORMATION($,$,#15174,#15515);
#214=ITEM_DEFINED_TRANSFORMATION($,$,#15174,#15516);
#215=ITEM_DEFINED_TRANSFORMATION($,$,#15174,#15517);
#216=ITEM_DEFINED_TRANSFORMATION($,$,#15174,#15518);
#217=ITEM_DEFINED_TRANSFORMATION($,$,#15415,#15519);
#218=ITEM_DEFINED_TRANSFORMATION($,$,#15415,#15520);
#219=ITEM_DEFINED_TRANSFORMATION($,$,#15415,#15521);
#220=ITEM_DEFINED_TRANSFORMATION($,$,#15415,#15522);
#221=ITEM_DEFINED_TRANSFORMATION($,$,#15199,#15569);
#222=ITEM_DEFINED_TRANSFORMATION($,$,#15235,#15570);
#223=ITEM_DEFINED_TRANSFORMATION($,$,#15244,#15571);
#224=ITEM_DEFINED_TRANSFORMATION($,$,#15253,#15572);
#225=ITEM_DEFINED_TRANSFORMATION($,$,#15262,#15573);
#226=ITEM_DEFINED_TRANSFORMATION($,$,#15271,#15574);
#227=ITEM_DEFINED_TRANSFORMATION($,$,#15280,#15575);
#228=ITEM_DEFINED_TRANSFORMATION($,$,#15289,#15576);
#229=ITEM_DEFINED_TRANSFORMATION($,$,#15313,#15577);
#230=ITEM_DEFINED_TRANSFORMATION($,$,#15322,#15578);
#231=ITEM_DEFINED_TRANSFORMATION($,$,#15523,#15579);
#232=ITEM_DEFINED_TRANSFORMATION($,$,#15415,#15580);
#233=ITEM_DEFINED_TRANSFORMATION($,$,#15415,#15581);
#234=ITEM_DEFINED_TRANSFORMATION($,$,#15523,#15582);
#235=ITEM_DEFINED_TRANSFORMATION($,$,#15534,#15583);
#236=ITEM_DEFINED_TRANSFORMATION($,$,#15543,#15584);
#237=ITEM_DEFINED_TRANSFORMATION($,$,#15586,#15595);
#238=ITEM_DEFINED_TRANSFORMATION($,$,#14318,#15596);
#239=ITEM_DEFINED_TRANSFORMATION($,$,#14930,#15597);
#240=ITEM_DEFINED_TRANSFORMATION($,$,#15198,#15598);
#241=ITEM_DEFINED_TRANSFORMATION($,$,#15585,#15599);
#242=(
REPRESENTATION_RELATIONSHIP($,$,#35095,#35094)
REPRESENTATION_RELATIONSHIP_WITH_TRANSFORMATION(#131)
SHAPE_REPRESENTATION_RELATIONSHIP()
);
#243=(
REPRESENTATION_RELATIONSHIP($,$,#35096,#35094)
REPRESENTATION_RELATIONSHIP_WITH_TRANSFORMATION(#132)
SHAPE_REPRESENTATION_RELATIONSHIP()
);
#244=(
REPRESENTATION_RELATIONSHIP($,$,#35097,#35094)
REPRESENTATION_RELATIONSHIP_WITH_TRANSFORMATION(#133)
SHAPE_REPRESENTATION_RELATIONSHIP()
);
#245=(
REPRESENTATION_RELATIONSHIP($,$,#35098,#35094)
REPRESENTATION_RELATIONSHIP_WITH_TRANSFORMATION(#134)
SHAPE_REPRESENTATION_RELATIONSHIP()
);
#246=(
REPRESENTATION_RELATIONSHIP($,$,#35099,#35094)
REPRESENTATION_RELATIONSHIP_WITH_TRANSFORMATION(#135)
SHAPE_REPRESENTATION_RELATIONSHIP()
);
#247=(
REPRESENTATION_RELATIONSHIP($,$,#35105,#35104)
REPRESENTATION_RELATIONSHIP_WITH_TRANSFORMATION(#136)
SHAPE_REPRESENTATION_RELATIONSHIP()
);
#248=(
REPRESENTATION_RELATIONSHIP($,$,#35106,#35104)
REPRESENTATION_RELATIONSHIP_WITH_TRANSFORMATION(#137)
SHAPE_REPRESENTATION_RELATIONSHIP()
);
#249=(
REPRESENTATION_RELATIONSHIP($,$,#35107,#35104)
REPRESENTATION_RELATIONSHIP_WITH_TRANSFORMATION(#138)
SHAPE_REPRESENTATION_RELATIONSHIP()
);
#250=(
REPRESENTATION_RELATIONSHIP($,$,#35075,#35074)
REPRESENTATION_RELATIONSHIP_WITH_TRANSFORMATION(#139)
SHAPE_REPRESENTATION_RELATIONSHIP()
);
#251=(
REPRESENTATION_RELATIONSHIP($,$,#35076,#35074)
REPRESENTATION_RELATIONSHIP_WITH_TRANSFORMATION(#140)
SHAPE_REPRESENTATION_RELATIONSHIP()
);
#252=(
REPRESENTATION_RELATIONSHIP($,$,#35077,#35074)
REPRESENTATION_RELATIONSHIP_WITH_TRANSFORMATION(#141)
SHAPE_REPRESENTATION_RELATIONSHIP()
);
#253=(
REPRESENTATION_RELATIONSHIP($,$,#35078,#35074)
REPRESENTATION_RELATIONSHIP_WITH_TRANSFORMATION(#142)
SHAPE_REPRESENTATION_RELATIONSHIP()
);
#254=(
REPRESENTATION_RELATIONSHIP($,$,#35079,#35074)
REPRESENTATION_RELATIONSHIP_WITH_TRANSFORMATION(#143)
SHAPE_REPRESENTATION_RELATIONSHIP()
);
#255=(
REPRESENTATION_RELATIONSHIP($,$,#35080,#35074)
REPRESENTATION_RELATIONSHIP_WITH_TRANSFORMATION(#144)
SHAPE_REPRESENTATION_RELATIONSHIP()
);
#256=(
REPRESENTATION_RELATIONSHIP($,$,#35081,#35074)
REPRESENTATION_RELATIONSHIP_WITH_TRANSFORMATION(#145)
SHAPE_REPRESENTATION_RELATIONSHIP()
);
#257=(
REPRESENTATION_RELATIONSHIP($,$,#35082,#35074)
REPRESENTATION_RELATIONSHIP_WITH_TRANSFORMATION(#146)
SHAPE_REPRESENTATION_RELATIONSHIP()
);
#258=(
REPRESENTATION_RELATIONSHIP($,$,#35083,#35074)
REPRESENTATION_RELATIONSHIP_WITH_TRANSFORMATION(#147)
SHAPE_REPRESENTATION_RELATIONSHIP()
);
#259=(
REPRESENTATION_RELATIONSHIP($,$,#35084,#35074)
REPRESENTATION_RELATIONSHIP_WITH_TRANSFORMATION(#148)
SHAPE_REPRESENTATION_RELATIONSHIP()
);
#260=(
REPRESENTATION_RELATIONSHIP($,$,#35085,#35074)
REPRESENTATION_RELATIONSHIP_WITH_TRANSFORMATION(#149)
SHAPE_REPRESENTATION_RELATIONSHIP()
);
#261=(
REPRESENTATION_RELATIONSHIP($,$,#35086,#35074)
REPRESENTATION_RELATIONSHIP_WITH_TRANSFORMATION(#150)
SHAPE_REPRESENTATION_RELATIONSHIP()
);
#262=(
REPRESENTATION_RELATIONSHIP($,$,#35087,#35074)
REPRESENTATION_RELATIONSHIP_WITH_TRANSFORMATION(#151)
SHAPE_REPRESENTATION_RELATIONSHIP()
);
#263=(
REPRESENTATION_RELATIONSHIP($,$,#35088,#35074)
REPRESENTATION_RELATIONSHIP_WITH_TRANSFORMATION(#152)
SHAPE_REPRESENTATION_RELATIONSHIP()
);
#264=(
REPRESENTATION_RELATIONSHIP($,$,#35089,#35074)
REPRESENTATION_RELATIONSHIP_WITH_TRANSFORMATION(#153)
SHAPE_REPRESENTATION_RELATIONSHIP()
);
#265=(
REPRESENTATION_RELATIONSHIP($,$,#35089,#35074)
REPRESENTATION_RELATIONSHIP_WITH_TRANSFORMATION(#154)
SHAPE_REPRESENTATION_RELATIONSHIP()
);
#266=(
REPRESENTATION_RELATIONSHIP($,$,#35090,#35074)
REPRESENTATION_RELATIONSHIP_WITH_TRANSFORMATION(#155)
SHAPE_REPRESENTATION_RELATIONSHIP()
);
#267=(
REPRESENTATION_RELATIONSHIP($,$,#35091,#35074)
REPRESENTATION_RELATIONSHIP_WITH_TRANSFORMATION(#156)
SHAPE_REPRESENTATION_RELATIONSHIP()
);
#268=(
REPRESENTATION_RELATIONSHIP($,$,#35108,#35074)
REPRESENTATION_RELATIONSHIP_WITH_TRANSFORMATION(#157)
SHAPE_REPRESENTATION_RELATIONSHIP()
);
#269=(
REPRESENTATION_RELATIONSHIP($,$,#35090,#35074)
REPRESENTATION_RELATIONSHIP_WITH_TRANSFORMATION(#158)
SHAPE_REPRESENTATION_RELATIONSHIP()
);
#270=(
REPRESENTATION_RELATIONSHIP($,$,#35091,#35074)
REPRESENTATION_RELATIONSHIP_WITH_TRANSFORMATION(#159)
SHAPE_REPRESENTATION_RELATIONSHIP()
);
#271=(
REPRESENTATION_RELATIONSHIP($,$,#35108,#35074)
REPRESENTATION_RELATIONSHIP_WITH_TRANSFORMATION(#160)
SHAPE_REPRESENTATION_RELATIONSHIP()
);
#272=(
REPRESENTATION_RELATIONSHIP($,$,#35090,#35074)
REPRESENTATION_RELATIONSHIP_WITH_TRANSFORMATION(#161)
SHAPE_REPRESENTATION_RELATIONSHIP()
);
#273=(
REPRESENTATION_RELATIONSHIP($,$,#35091,#35074)
REPRESENTATION_RELATIONSHIP_WITH_TRANSFORMATION(#162)
SHAPE_REPRESENTATION_RELATIONSHIP()
);
#274=(
REPRESENTATION_RELATIONSHIP($,$,#35108,#35074)
REPRESENTATION_RELATIONSHIP_WITH_TRANSFORMATION(#163)
SHAPE_REPRESENTATION_RELATIONSHIP()
);
#275=(
REPRESENTATION_RELATIONSHIP($,$,#35090,#35074)
REPRESENTATION_RELATIONSHIP_WITH_TRANSFORMATION(#164)
SHAPE_REPRESENTATION_RELATIONSHIP()
);
#276=(
REPRESENTATION_RELATIONSHIP($,$,#35091,#35074)
REPRESENTATION_RELATIONSHIP_WITH_TRANSFORMATION(#165)
SHAPE_REPRESENTATION_RELATIONSHIP()
);
#277=(
REPRESENTATION_RELATIONSHIP($,$,#35108,#35074)
REPRESENTATION_RELATIONSHIP_WITH_TRANSFORMATION(#166)
SHAPE_REPRESENTATION_RELATIONSHIP()
);
#278=(
REPRESENTATION_RELATIONSHIP($,$,#35090,#35074)
REPRESENTATION_RELATIONSHIP_WITH_TRANSFORMATION(#167)
SHAPE_REPRESENTATION_RELATIONSHIP()
);
#279=(
REPRESENTATION_RELATIONSHIP($,$,#35091,#35074)
REPRESENTATION_RELATIONSHIP_WITH_TRANSFORMATION(#168)
SHAPE_REPRESENTATION_RELATIONSHIP()
);
#280=(
REPRESENTATION_RELATIONSHIP($,$,#35108,#35074)
REPRESENTATION_RELATIONSHIP_WITH_TRANSFORMATION(#169)
SHAPE_REPRESENTATION_RELATIONSHIP()
);
#281=(
REPRESENTATION_RELATIONSHIP($,$,#35090,#35074)
REPRESENTATION_RELATIONSHIP_WITH_TRANSFORMATION(#170)
SHAPE_REPRESENTATION_RELATIONSHIP()
);
#282=(
REPRESENTATION_RELATIONSHIP($,$,#35091,#35074)
REPRESENTATION_RELATIONSHIP_WITH_TRANSFORMATION(#171)
SHAPE_REPRESENTATION_RELATIONSHIP()
);
#283=(
REPRESENTATION_RELATIONSHIP($,$,#35108,#35074)
REPRESENTATION_RELATIONSHIP_WITH_TRANSFORMATION(#172)
SHAPE_REPRESENTATION_RELATIONSHIP()
);
#284=(
REPRESENTATION_RELATIONSHIP($,$,#35090,#35074)
REPRESENTATION_RELATIONSHIP_WITH_TRANSFORMATION(#173)
SHAPE_REPRESENTATION_RELATIONSHIP()
);
#285=(
REPRESENTATION_RELATIONSHIP($,$,#35091,#35074)
REPRESENTATION_RELATIONSHIP_WITH_TRANSFORMATION(#174)
SHAPE_REPRESENTATION_RELATIONSHIP()
);
#286=(
REPRESENTATION_RELATIONSHIP($,$,#35108,#35074)
REPRESENTATION_RELATIONSHIP_WITH_TRANSFORMATION(#175)
SHAPE_REPRESENTATION_RELATIONSHIP()
);
#287=(
REPRESENTATION_RELATIONSHIP($,$,#35090,#35074)
REPRESENTATION_RELATIONSHIP_WITH_TRANSFORMATION(#176)
SHAPE_REPRESENTATION_RELATIONSHIP()
);
#288=(
REPRESENTATION_RELATIONSHIP($,$,#35091,#35074)
REPRESENTATION_RELATIONSHIP_WITH_TRANSFORMATION(#177)
SHAPE_REPRESENTATION_RELATIONSHIP()
);
#289=(
REPRESENTATION_RELATIONSHIP($,$,#35108,#35074)
REPRESENTATION_RELATIONSHIP_WITH_TRANSFORMATION(#178)
SHAPE_REPRESENTATION_RELATIONSHIP()
);
#290=(
REPRESENTATION_RELATIONSHIP($,$,#35092,#35074)
REPRESENTATION_RELATIONSHIP_WITH_TRANSFORMATION(#179)
SHAPE_REPRESENTATION_RELATIONSHIP()
);
#291=(
REPRESENTATION_RELATIONSHIP($,$,#35120,#35074)
REPRESENTATION_RELATIONSHIP_WITH_TRANSFORMATION(#180)
SHAPE_REPRESENTATION_RELATIONSHIP()
);
#292=(
REPRESENTATION_RELATIONSHIP($,$,#35120,#35074)
REPRESENTATION_RELATIONSHIP_WITH_TRANSFORMATION(#181)
SHAPE_REPRESENTATION_RELATIONSHIP()
);
#293=(
REPRESENTATION_RELATIONSHIP($,$,#35120,#35074)
REPRESENTATION_RELATIONSHIP_WITH_TRANSFORMATION(#182)
SHAPE_REPRESENTATION_RELATIONSHIP()
);
#294=(
REPRESENTATION_RELATIONSHIP($,$,#35120,#35074)
REPRESENTATION_RELATIONSHIP_WITH_TRANSFORMATION(#183)
SHAPE_REPRESENTATION_RELATIONSHIP()
);
#295=(
REPRESENTATION_RELATIONSHIP($,$,#35093,#35074)
REPRESENTATION_RELATIONSHIP_WITH_TRANSFORMATION(#184)
SHAPE_REPRESENTATION_RELATIONSHIP()
);
#296=(
REPRESENTATION_RELATIONSHIP($,$,#35093,#35074)
REPRESENTATION_RELATIONSHIP_WITH_TRANSFORMATION(#185)
SHAPE_REPRESENTATION_RELATIONSHIP()
);
#297=(
REPRESENTATION_RELATIONSHIP($,$,#35093,#35074)
REPRESENTATION_RELATIONSHIP_WITH_TRANSFORMATION(#186)
SHAPE_REPRESENTATION_RELATIONSHIP()
);
#298=(
REPRESENTATION_RELATIONSHIP($,$,#35093,#35074)
REPRESENTATION_RELATIONSHIP_WITH_TRANSFORMATION(#187)
SHAPE_REPRESENTATION_RELATIONSHIP()
);
#299=(
REPRESENTATION_RELATIONSHIP($,$,#35120,#35074)
REPRESENTATION_RELATIONSHIP_WITH_TRANSFORMATION(#188)
SHAPE_REPRESENTATION_RELATIONSHIP()
);
#300=(
REPRESENTATION_RELATIONSHIP($,$,#35120,#35074)
REPRESENTATION_RELATIONSHIP_WITH_TRANSFORMATION(#189)
SHAPE_REPRESENTATION_RELATIONSHIP()
);
#301=(
REPRESENTATION_RELATIONSHIP($,$,#35094,#35074)
REPRESENTATION_RELATIONSHIP_WITH_TRANSFORMATION(#190)
SHAPE_REPRESENTATION_RELATIONSHIP()
);
#302=(
REPRESENTATION_RELATIONSHIP($,$,#35100,#35074)
REPRESENTATION_RELATIONSHIP_WITH_TRANSFORMATION(#191)
SHAPE_REPRESENTATION_RELATIONSHIP()
);
#303=(
REPRESENTATION_RELATIONSHIP($,$,#35100,#35074)
REPRESENTATION_RELATIONSHIP_WITH_TRANSFORMATION(#192)
SHAPE_REPRESENTATION_RELATIONSHIP()
);
#304=(
REPRESENTATION_RELATIONSHIP($,$,#35100,#35074)
REPRESENTATION_RELATIONSHIP_WITH_TRANSFORMATION(#193)
SHAPE_REPRESENTATION_RELATIONSHIP()
);
#305=(
REPRESENTATION_RELATIONSHIP($,$,#35100,#35074)
REPRESENTATION_RELATIONSHIP_WITH_TRANSFORMATION(#194)
SHAPE_REPRESENTATION_RELATIONSHIP()
);
#306=(
REPRESENTATION_RELATIONSHIP($,$,#35100,#35074)
REPRESENTATION_RELATIONSHIP_WITH_TRANSFORMATION(#195)
SHAPE_REPRESENTATION_RELATIONSHIP()
);
#307=(
REPRESENTATION_RELATIONSHIP($,$,#35100,#35074)
REPRESENTATION_RELATIONSHIP_WITH_TRANSFORMATION(#196)
SHAPE_REPRESENTATION_RELATIONSHIP()
);
#308=(
REPRESENTATION_RELATIONSHIP($,$,#35100,#35074)
REPRESENTATION_RELATIONSHIP_WITH_TRANSFORMATION(#197)
SHAPE_REPRESENTATION_RELATIONSHIP()
);
#309=(
REPRESENTATION_RELATIONSHIP($,$,#35100,#35074)
REPRESENTATION_RELATIONSHIP_WITH_TRANSFORMATION(#198)
SHAPE_REPRESENTATION_RELATIONSHIP()
);
#310=(
REPRESENTATION_RELATIONSHIP($,$,#35120,#35074)
REPRESENTATION_RELATIONSHIP_WITH_TRANSFORMATION(#199)
SHAPE_REPRESENTATION_RELATIONSHIP()
);
#311=(
REPRESENTATION_RELATIONSHIP($,$,#35120,#35074)
REPRESENTATION_RELATIONSHIP_WITH_TRANSFORMATION(#200)
SHAPE_REPRESENTATION_RELATIONSHIP()
);
#312=(
REPRESENTATION_RELATIONSHIP($,$,#35094,#35074)
REPRESENTATION_RELATIONSHIP_WITH_TRANSFORMATION(#201)
SHAPE_REPRESENTATION_RELATIONSHIP()
);
#313=(
REPRESENTATION_RELATIONSHIP($,$,#35100,#35074)
REPRESENTATION_RELATIONSHIP_WITH_TRANSFORMATION(#202)
SHAPE_REPRESENTATION_RELATIONSHIP()
);
#314=(
REPRESENTATION_RELATIONSHIP($,$,#35100,#35074)
REPRESENTATION_RELATIONSHIP_WITH_TRANSFORMATION(#203)
SHAPE_REPRESENTATION_RELATIONSHIP()
);
#315=(
REPRESENTATION_RELATIONSHIP($,$,#35100,#35074)
REPRESENTATION_RELATIONSHIP_WITH_TRANSFORMATION(#204)
SHAPE_REPRESENTATION_RELATIONSHIP()
);
#316=(
REPRESENTATION_RELATIONSHIP($,$,#35100,#35074)
REPRESENTATION_RELATIONSHIP_WITH_TRANSFORMATION(#205)
SHAPE_REPRESENTATION_RELATIONSHIP()
);
#317=(
REPRESENTATION_RELATIONSHIP($,$,#35100,#35074)
REPRESENTATION_RELATIONSHIP_WITH_TRANSFORMATION(#206)
SHAPE_REPRESENTATION_RELATIONSHIP()
);
#318=(
REPRESENTATION_RELATIONSHIP($,$,#35100,#35074)
REPRESENTATION_RELATIONSHIP_WITH_TRANSFORMATION(#207)
SHAPE_REPRESENTATION_RELATIONSHIP()
);
#319=(
REPRESENTATION_RELATIONSHIP($,$,#35100,#35074)
REPRESENTATION_RELATIONSHIP_WITH_TRANSFORMATION(#208)
SHAPE_REPRESENTATION_RELATIONSHIP()
);
#320=(
REPRESENTATION_RELATIONSHIP($,$,#35100,#35074)
REPRESENTATION_RELATIONSHIP_WITH_TRANSFORMATION(#209)
SHAPE_REPRESENTATION_RELATIONSHIP()
);
#321=(
REPRESENTATION_RELATIONSHIP($,$,#35102,#35101)
REPRESENTATION_RELATIONSHIP_WITH_TRANSFORMATION(#210)
SHAPE_REPRESENTATION_RELATIONSHIP()
);
#322=(
REPRESENTATION_RELATIONSHIP($,$,#35103,#35101)
REPRESENTATION_RELATIONSHIP_WITH_TRANSFORMATION(#211)
SHAPE_REPRESENTATION_RELATIONSHIP()
);
#323=(
REPRESENTATION_RELATIONSHIP($,$,#35104,#35101)
REPRESENTATION_RELATIONSHIP_WITH_TRANSFORMATION(#212)
SHAPE_REPRESENTATION_RELATIONSHIP()
);
#324=(
REPRESENTATION_RELATIONSHIP($,$,#35108,#35101)
REPRESENTATION_RELATIONSHIP_WITH_TRANSFORMATION(#213)
SHAPE_REPRESENTATION_RELATIONSHIP()
);
#325=(
REPRESENTATION_RELATIONSHIP($,$,#35108,#35101)
REPRESENTATION_RELATIONSHIP_WITH_TRANSFORMATION(#214)
SHAPE_REPRESENTATION_RELATIONSHIP()
);
#326=(
REPRESENTATION_RELATIONSHIP($,$,#35108,#35101)
REPRESENTATION_RELATIONSHIP_WITH_TRANSFORMATION(#215)
SHAPE_REPRESENTATION_RELATIONSHIP()
);
#327=(
REPRESENTATION_RELATIONSHIP($,$,#35108,#35101)
REPRESENTATION_RELATIONSHIP_WITH_TRANSFORMATION(#216)
SHAPE_REPRESENTATION_RELATIONSHIP()
);
#328=(
REPRESENTATION_RELATIONSHIP($,$,#35120,#35101)
REPRESENTATION_RELATIONSHIP_WITH_TRANSFORMATION(#217)
SHAPE_REPRESENTATION_RELATIONSHIP()
);
#329=(
REPRESENTATION_RELATIONSHIP($,$,#35120,#35101)
REPRESENTATION_RELATIONSHIP_WITH_TRANSFORMATION(#218)
SHAPE_REPRESENTATION_RELATIONSHIP()
);
#330=(
REPRESENTATION_RELATIONSHIP($,$,#35120,#35101)
REPRESENTATION_RELATIONSHIP_WITH_TRANSFORMATION(#219)
SHAPE_REPRESENTATION_RELATIONSHIP()
);
#331=(
REPRESENTATION_RELATIONSHIP($,$,#35120,#35101)
REPRESENTATION_RELATIONSHIP_WITH_TRANSFORMATION(#220)
SHAPE_REPRESENTATION_RELATIONSHIP()
);
#332=(
REPRESENTATION_RELATIONSHIP($,$,#35110,#35109)
REPRESENTATION_RELATIONSHIP_WITH_TRANSFORMATION(#221)
SHAPE_REPRESENTATION_RELATIONSHIP()
);
#333=(
REPRESENTATION_RELATIONSHIP($,$,#35111,#35109)
REPRESENTATION_RELATIONSHIP_WITH_TRANSFORMATION(#222)
SHAPE_REPRESENTATION_RELATIONSHIP()
);
#334=(
REPRESENTATION_RELATIONSHIP($,$,#35112,#35109)
REPRESENTATION_RELATIONSHIP_WITH_TRANSFORMATION(#223)
SHAPE_REPRESENTATION_RELATIONSHIP()
);
#335=(
REPRESENTATION_RELATIONSHIP($,$,#35113,#35109)
REPRESENTATION_RELATIONSHIP_WITH_TRANSFORMATION(#224)
SHAPE_REPRESENTATION_RELATIONSHIP()
);
#336=(
REPRESENTATION_RELATIONSHIP($,$,#35114,#35109)
REPRESENTATION_RELATIONSHIP_WITH_TRANSFORMATION(#225)
SHAPE_REPRESENTATION_RELATIONSHIP()
);
#337=(
REPRESENTATION_RELATIONSHIP($,$,#35115,#35109)
REPRESENTATION_RELATIONSHIP_WITH_TRANSFORMATION(#226)
SHAPE_REPRESENTATION_RELATIONSHIP()
);
#338=(
REPRESENTATION_RELATIONSHIP($,$,#35116,#35109)
REPRESENTATION_RELATIONSHIP_WITH_TRANSFORMATION(#227)
SHAPE_REPRESENTATION_RELATIONSHIP()
);
#339=(
REPRESENTATION_RELATIONSHIP($,$,#35117,#35109)
REPRESENTATION_RELATIONSHIP_WITH_TRANSFORMATION(#228)
SHAPE_REPRESENTATION_RELATIONSHIP()
);
#340=(
REPRESENTATION_RELATIONSHIP($,$,#35118,#35109)
REPRESENTATION_RELATIONSHIP_WITH_TRANSFORMATION(#229)
SHAPE_REPRESENTATION_RELATIONSHIP()
);
#341=(
REPRESENTATION_RELATIONSHIP($,$,#35119,#35109)
REPRESENTATION_RELATIONSHIP_WITH_TRANSFORMATION(#230)
SHAPE_REPRESENTATION_RELATIONSHIP()
);
#342=(
REPRESENTATION_RELATIONSHIP($,$,#35121,#35109)
REPRESENTATION_RELATIONSHIP_WITH_TRANSFORMATION(#231)
SHAPE_REPRESENTATION_RELATIONSHIP()
);
#343=(
REPRESENTATION_RELATIONSHIP($,$,#35120,#35109)
REPRESENTATION_RELATIONSHIP_WITH_TRANSFORMATION(#232)
SHAPE_REPRESENTATION_RELATIONSHIP()
);
#344=(
REPRESENTATION_RELATIONSHIP($,$,#35120,#35109)
REPRESENTATION_RELATIONSHIP_WITH_TRANSFORMATION(#233)
SHAPE_REPRESENTATION_RELATIONSHIP()
);
#345=(
REPRESENTATION_RELATIONSHIP($,$,#35121,#35109)
REPRESENTATION_RELATIONSHIP_WITH_TRANSFORMATION(#234)
SHAPE_REPRESENTATION_RELATIONSHIP()
);
#346=(
REPRESENTATION_RELATIONSHIP($,$,#35122,#35109)
REPRESENTATION_RELATIONSHIP_WITH_TRANSFORMATION(#235)
SHAPE_REPRESENTATION_RELATIONSHIP()
);
#347=(
REPRESENTATION_RELATIONSHIP($,$,#35123,#35109)
REPRESENTATION_RELATIONSHIP_WITH_TRANSFORMATION(#236)
SHAPE_REPRESENTATION_RELATIONSHIP()
);
#348=(
REPRESENTATION_RELATIONSHIP($,$,#35125,#35124)
REPRESENTATION_RELATIONSHIP_WITH_TRANSFORMATION(#237)
SHAPE_REPRESENTATION_RELATIONSHIP()
);
#349=(
REPRESENTATION_RELATIONSHIP($,$,#35074,#35073)
REPRESENTATION_RELATIONSHIP_WITH_TRANSFORMATION(#238)
SHAPE_REPRESENTATION_RELATIONSHIP()
);
#350=(
REPRESENTATION_RELATIONSHIP($,$,#35101,#35073)
REPRESENTATION_RELATIONSHIP_WITH_TRANSFORMATION(#239)
SHAPE_REPRESENTATION_RELATIONSHIP()
);
#351=(
REPRESENTATION_RELATIONSHIP($,$,#35109,#35073)
REPRESENTATION_RELATIONSHIP_WITH_TRANSFORMATION(#240)
SHAPE_REPRESENTATION_RELATIONSHIP()
);
#352=(
REPRESENTATION_RELATIONSHIP($,$,#35124,#35073)
REPRESENTATION_RELATIONSHIP_WITH_TRANSFORMATION(#241)
SHAPE_REPRESENTATION_RELATIONSHIP()
);
#353=CONTEXT_DEPENDENT_SHAPE_REPRESENTATION(#242,#34936);
#354=CONTEXT_DEPENDENT_SHAPE_REPRESENTATION(#243,#34937);
#355=CONTEXT_DEPENDENT_SHAPE_REPRESENTATION(#244,#34938);
#356=CONTEXT_DEPENDENT_SHAPE_REPRESENTATION(#245,#34939);
#357=CONTEXT_DEPENDENT_SHAPE_REPRESENTATION(#246,#34940);
#358=CONTEXT_DEPENDENT_SHAPE_REPRESENTATION(#247,#34949);
#359=CONTEXT_DEPENDENT_SHAPE_REPRESENTATION(#248,#34950);
#360=CONTEXT_DEPENDENT_SHAPE_REPRESENTATION(#249,#34951);
#361=CONTEXT_DEPENDENT_SHAPE_REPRESENTATION(#250,#34965);
#362=CONTEXT_DEPENDENT_SHAPE_REPRESENTATION(#251,#34966);
#363=CONTEXT_DEPENDENT_SHAPE_REPRESENTATION(#252,#34967);
#364=CONTEXT_DEPENDENT_SHAPE_REPRESENTATION(#253,#34968);
#365=CONTEXT_DEPENDENT_SHAPE_REPRESENTATION(#254,#34969);
#366=CONTEXT_DEPENDENT_SHAPE_REPRESENTATION(#255,#34970);
#367=CONTEXT_DEPENDENT_SHAPE_REPRESENTATION(#256,#34971);
#368=CONTEXT_DEPENDENT_SHAPE_REPRESENTATION(#257,#34972);
#369=CONTEXT_DEPENDENT_SHAPE_REPRESENTATION(#258,#34973);
#370=CONTEXT_DEPENDENT_SHAPE_REPRESENTATION(#259,#34974);
#371=CONTEXT_DEPENDENT_SHAPE_REPRESENTATION(#260,#34975);
#372=CONTEXT_DEPENDENT_SHAPE_REPRESENTATION(#261,#34976);
#373=CONTEXT_DEPENDENT_SHAPE_REPRESENTATION(#262,#34977);
#374=CONTEXT_DEPENDENT_SHAPE_REPRESENTATION(#263,#34978);
#375=CONTEXT_DEPENDENT_SHAPE_REPRESENTATION(#264,#34979);
#376=CONTEXT_DEPENDENT_SHAPE_REPRESENTATION(#265,#34980);
#377=CONTEXT_DEPENDENT_SHAPE_REPRESENTATION(#266,#34981);
#378=CONTEXT_DEPENDENT_SHAPE_REPRESENTATION(#267,#34982);
#379=CONTEXT_DEPENDENT_SHAPE_REPRESENTATION(#268,#34983);
#380=CONTEXT_DEPENDENT_SHAPE_REPRESENTATION(#269,#34984);
#381=CONTEXT_DEPENDENT_SHAPE_REPRESENTATION(#270,#34985);
#382=CONTEXT_DEPENDENT_SHAPE_REPRESENTATION(#271,#34986);
#383=CONTEXT_DEPENDENT_SHAPE_REPRESENTATION(#272,#34987);
#384=CONTEXT_DEPENDENT_SHAPE_REPRESENTATION(#273,#34988);
#385=CONTEXT_DEPENDENT_SHAPE_REPRESENTATION(#274,#34989);
#386=CONTEXT_DEPENDENT_SHAPE_REPRESENTATION(#275,#34990);
#387=CONTEXT_DEPENDENT_SHAPE_REPRESENTATION(#276,#34991);
#388=CONTEXT_DEPENDENT_SHAPE_REPRESENTATION(#277,#34992);
#389=CONTEXT_DEPENDENT_SHAPE_REPRESENTATION(#278,#34993);
#390=CONTEXT_DEPENDENT_SHAPE_REPRESENTATION(#279,#34994);
#391=CONTEXT_DEPENDENT_SHAPE_REPRESENTATION(#280,#34995);
#392=CONTEXT_DEPENDENT_SHAPE_REPRESENTATION(#281,#34996);
#393=CONTEXT_DEPENDENT_SHAPE_REPRESENTATION(#282,#34997);
#394=CONTEXT_DEPENDENT_SHAPE_REPRESENTATION(#283,#34998);
#395=CONTEXT_DEPENDENT_SHAPE_REPRESENTATION(#284,#34999);
#396=CONTEXT_DEPENDENT_SHAPE_REPRESENTATION(#285,#35000);
#397=CONTEXT_DEPENDENT_SHAPE_REPRESENTATION(#286,#35001);
#398=CONTEXT_DEPENDENT_SHAPE_REPRESENTATION(#287,#35002);
#399=CONTEXT_DEPENDENT_SHAPE_REPRESENTATION(#288,#35003);
#400=CONTEXT_DEPENDENT_SHAPE_REPRESENTATION(#289,#35004);
#401=CONTEXT_DEPENDENT_SHAPE_REPRESENTATION(#290,#35005);
#402=CONTEXT_DEPENDENT_SHAPE_REPRESENTATION(#291,#35006);
#403=CONTEXT_DEPENDENT_SHAPE_REPRESENTATION(#292,#35007);
#404=CONTEXT_DEPENDENT_SHAPE_REPRESENTATION(#293,#35008);
#405=CONTEXT_DEPENDENT_SHAPE_REPRESENTATION(#294,#35009);
#406=CONTEXT_DEPENDENT_SHAPE_REPRESENTATION(#295,#35010);
#407=CONTEXT_DEPENDENT_SHAPE_REPRESENTATION(#296,#35011);
#408=CONTEXT_DEPENDENT_SHAPE_REPRESENTATION(#297,#35012);
#409=CONTEXT_DEPENDENT_SHAPE_REPRESENTATION(#298,#35013);
#410=CONTEXT_DEPENDENT_SHAPE_REPRESENTATION(#299,#35014);
#411=CONTEXT_DEPENDENT_SHAPE_REPRESENTATION(#300,#35015);
#412=CONTEXT_DEPENDENT_SHAPE_REPRESENTATION(#301,#35016);
#413=CONTEXT_DEPENDENT_SHAPE_REPRESENTATION(#302,#35017);
#414=CONTEXT_DEPENDENT_SHAPE_REPRESENTATION(#303,#35018);
#415=CONTEXT_DEPENDENT_SHAPE_REPRESENTATION(#304,#35019);
#416=CONTEXT_DEPENDENT_SHAPE_REPRESENTATION(#305,#35020);
#417=CONTEXT_DEPENDENT_SHAPE_REPRESENTATION(#306,#35021);
#418=CONTEXT_DEPENDENT_SHAPE_REPRESENTATION(#307,#35022);
#419=CONTEXT_DEPENDENT_SHAPE_REPRESENTATION(#308,#35023);
#420=CONTEXT_DEPENDENT_SHAPE_REPRESENTATION(#309,#35024);
#421=CONTEXT_DEPENDENT_SHAPE_REPRESENTATION(#310,#35025);
#422=CONTEXT_DEPENDENT_SHAPE_REPRESENTATION(#311,#35026);
#423=CONTEXT_DEPENDENT_SHAPE_REPRESENTATION(#312,#35027);
#424=CONTEXT_DEPENDENT_SHAPE_REPRESENTATION(#313,#35028);
#425=CONTEXT_DEPENDENT_SHAPE_REPRESENTATION(#314,#35029);
#426=CONTEXT_DEPENDENT_SHAPE_REPRESENTATION(#315,#35030);
#427=CONTEXT_DEPENDENT_SHAPE_REPRESENTATION(#316,#35031);
#428=CONTEXT_DEPENDENT_SHAPE_REPRESENTATION(#317,#35032);
#429=CONTEXT_DEPENDENT_SHAPE_REPRESENTATION(#318,#35033);
#430=CONTEXT_DEPENDENT_SHAPE_REPRESENTATION(#319,#35034);
#431=CONTEXT_DEPENDENT_SHAPE_REPRESENTATION(#320,#35035);
#432=CONTEXT_DEPENDENT_SHAPE_REPRESENTATION(#321,#35036);
#433=CONTEXT_DEPENDENT_SHAPE_REPRESENTATION(#322,#35037);
#434=CONTEXT_DEPENDENT_SHAPE_REPRESENTATION(#323,#35038);
#435=CONTEXT_DEPENDENT_SHAPE_REPRESENTATION(#324,#35039);
#436=CONTEXT_DEPENDENT_SHAPE_REPRESENTATION(#325,#35040);
#437=CONTEXT_DEPENDENT_SHAPE_REPRESENTATION(#326,#35041);
#438=CONTEXT_DEPENDENT_SHAPE_REPRESENTATION(#327,#35042);
#439=CONTEXT_DEPENDENT_SHAPE_REPRESENTATION(#328,#35043);
#440=CONTEXT_DEPENDENT_SHAPE_REPRESENTATION(#329,#35044);
#441=CONTEXT_DEPENDENT_SHAPE_REPRESENTATION(#330,#35045);
#442=CONTEXT_DEPENDENT_SHAPE_REPRESENTATION(#331,#35046);
#443=CONTEXT_DEPENDENT_SHAPE_REPRESENTATION(#332,#35050);
#444=CONTEXT_DEPENDENT_SHAPE_REPRESENTATION(#333,#35051);
#445=CONTEXT_DEPENDENT_SHAPE_REPRESENTATION(#334,#35052);
#446=CONTEXT_DEPENDENT_SHAPE_REPRESENTATION(#335,#35053);
#447=CONTEXT_DEPENDENT_SHAPE_REPRESENTATION(#336,#35054);
#448=CONTEXT_DEPENDENT_SHAPE_REPRESENTATION(#337,#35055);
#449=CONTEXT_DEPENDENT_SHAPE_REPRESENTATION(#338,#35056);
#450=CONTEXT_DEPENDENT_SHAPE_REPRESENTATION(#339,#35057);
#451=CONTEXT_DEPENDENT_SHAPE_REPRESENTATION(#340,#35058);
#452=CONTEXT_DEPENDENT_SHAPE_REPRESENTATION(#341,#35059);
#453=CONTEXT_DEPENDENT_SHAPE_REPRESENTATION(#342,#35060);
#454=CONTEXT_DEPENDENT_SHAPE_REPRESENTATION(#343,#35061);
#455=CONTEXT_DEPENDENT_SHAPE_REPRESENTATION(#344,#35062);
#456=CONTEXT_DEPENDENT_SHAPE_REPRESENTATION(#345,#35063);
#457=CONTEXT_DEPENDENT_SHAPE_REPRESENTATION(#346,#35064);
#458=CONTEXT_DEPENDENT_SHAPE_REPRESENTATION(#347,#35065);
#459=CONTEXT_DEPENDENT_SHAPE_REPRESENTATION(#348,#35068);
#460=CONTEXT_DEPENDENT_SHAPE_REPRESENTATION(#349,#35069);
#461=CONTEXT_DEPENDENT_SHAPE_REPRESENTATION(#350,#35070);
#462=CONTEXT_DEPENDENT_SHAPE_REPRESENTATION(#351,#35071);
#463=CONTEXT_DEPENDENT_SHAPE_REPRESENTATION(#352,#35072);
#464=NEXT_ASSEMBLY_USAGE_OCCURRENCE('Inner ring:1','Inner ring:1',
'Inner ring:1',#35148,#35149,'Inner ring:1');
#465=NEXT_ASSEMBLY_USAGE_OCCURRENCE('Outer ring:1','Outer ring:1',
'Outer ring:1',#35148,#35150,'Outer ring:1');
#466=NEXT_ASSEMBLY_USAGE_OCCURRENCE('Balls:1','Balls:1','Balls:1',#35148,
#35151,'Balls:1');
#467=NEXT_ASSEMBLY_USAGE_OCCURRENCE('Cage:1','Cage:1','Cage:1',#35148,#35152,
'Cage:1');
#468=NEXT_ASSEMBLY_USAGE_OCCURRENCE('Seals 2RS:1','Seals 2RS:1',
'Seals 2RS:1',#35148,#35153,'Seals 2RS:1');
#469=NEXT_ASSEMBLY_USAGE_OCCURRENCE('Block:1','Block:1','Block:1',#35158,
#35159,'Block:1');
#470=NEXT_ASSEMBLY_USAGE_OCCURRENCE('End cap +:1','End cap +:1',
'End cap +:1',#35158,#35160,'End cap +:1');
#471=NEXT_ASSEMBLY_USAGE_OCCURRENCE('End cap:1','End cap:1','End cap:1',
#35158,#35161,'End cap:1');
#472=NEXT_ASSEMBLY_USAGE_OCCURRENCE('Base:1','Base:1','Base:1',#35128,#35129,
'Base:1');
#473=NEXT_ASSEMBLY_USAGE_OCCURRENCE('Foot strip:1','Foot strip:1',
'Foot strip:1',#35128,#35130,'Foot strip:1');
#474=NEXT_ASSEMBLY_USAGE_OCCURRENCE('Foot strip (1):1',
'Foot strip (1):1','Foot strip (1):1',#35128,#35131,'Foot strip (1):1');
#475=NEXT_ASSEMBLY_USAGE_OCCURRENCE('Rail support plate:1',
'Rail support plate:1','Rail support plate:1',#35128,#35132,
'Rail support plate:1');
#476=NEXT_ASSEMBLY_USAGE_OCCURRENCE('End stop:1','End stop:1',
'End stop:1',#35128,#35133,'End stop:1');
#477=NEXT_ASSEMBLY_USAGE_OCCURRENCE('End bumper:1','End bumper:1',
'End bumper:1',#35128,#35134,'End bumper:1');
#478=NEXT_ASSEMBLY_USAGE_OCCURRENCE('End stop (1):1','End stop (1):1',
'End stop (1):1',#35128,#35135,'End stop (1):1');
#479=NEXT_ASSEMBLY_USAGE_OCCURRENCE('End bumper (1):1',
'End bumper (1):1','End bumper (1):1',#35128,#35136,'End bumper (1):1');
#480=NEXT_ASSEMBLY_USAGE_OCCURRENCE('Pinion bearing pedestal:1',
'Pinion bearing pedestal:1','Pinion bearing pedestal:1',#35128,#35137,
'Pinion bearing pedestal:1');
#481=NEXT_ASSEMBLY_USAGE_OCCURRENCE('Bearing cap:1','Bearing cap:1',
'Bearing cap:1',#35128,#35138,'Bearing cap:1');
#482=NEXT_ASSEMBLY_USAGE_OCCURRENCE('Bearing cap (1):1',
'Bearing cap (1):1','Bearing cap (1):1',#35128,#35139,
'Bearing cap (1):1');
#483=NEXT_ASSEMBLY_USAGE_OCCURRENCE('Pinion bearing pedestal (1):1',
'Pinion bearing pedestal (1):1','Pinion bearing pedestal (1):1',#35128,
#35140,'Pinion bearing pedestal (1):1');
#484=NEXT_ASSEMBLY_USAGE_OCCURRENCE('Bearing cap (2):1',
'Bearing cap (2):1','Bearing cap (2):1',#35128,#35141,
'Bearing cap (2):1');
#485=NEXT_ASSEMBLY_USAGE_OCCURRENCE('Bearing cap (3):1',
'Bearing cap (3):1','Bearing cap (3):1',#35128,#35142,
'Bearing cap (3):1');
#486=NEXT_ASSEMBLY_USAGE_OCCURRENCE(
'Slotted Extrusion - 20 x 20 x 200 mm:2',
'Slotted Extrusion - 20 x 20 x 200 mm:2',
'Slotted Extrusion - 20 x 20 x 200 mm:2',#35128,#35143,
'Slotted Extrusion - 20 x 20 x 200 mm:2');
#487=NEXT_ASSEMBLY_USAGE_OCCURRENCE(
'Slotted Extrusion - 20 x 20 x 200 mm:3',
'Slotted Extrusion - 20 x 20 x 200 mm:3',
'Slotted Extrusion - 20 x 20 x 200 mm:3',#35128,#35143,
'Slotted Extrusion - 20 x 20 x 200 mm:3');
#488=NEXT_ASSEMBLY_USAGE_OCCURRENCE('Captive slot nut:2',
'Captive slot nut:2','Captive slot nut:2',#35128,#35144,
'Captive slot nut:2');
#489=NEXT_ASSEMBLY_USAGE_OCCURRENCE('Flat Washer - M5:2',
'Flat Washer - M5:2','Flat Washer - M5:2',#35128,#35145,
'Flat Washer - M5:2');
#490=NEXT_ASSEMBLY_USAGE_OCCURRENCE('M5x14 Cap Screw:2',
'M5x14 Cap Screw:2','M5x14 Cap Screw:2',#35128,#35162,
'M5x14 Cap Screw:2');
#491=NEXT_ASSEMBLY_USAGE_OCCURRENCE('Captive slot nut:3',
'Captive slot nut:3','Captive slot nut:3',#35128,#35144,
'Captive slot nut:3');
#492=NEXT_ASSEMBLY_USAGE_OCCURRENCE('Flat Washer - M5:3',
'Flat Washer - M5:3','Flat Washer - M5:3',#35128,#35145,
'Flat Washer - M5:3');
#493=NEXT_ASSEMBLY_USAGE_OCCURRENCE('M5x14 Cap Screw:3',
'M5x14 Cap Screw:3','M5x14 Cap Screw:3',#35128,#35162,
'M5x14 Cap Screw:3');
#494=NEXT_ASSEMBLY_USAGE_OCCURRENCE('Captive slot nut:4',
'Captive slot nut:4','Captive slot nut:4',#35128,#35144,
'Captive slot nut:4');
#495=NEXT_ASSEMBLY_USAGE_OCCURRENCE('Flat Washer - M5:4',
'Flat Washer - M5:4','Flat Washer - M5:4',#35128,#35145,
'Flat Washer - M5:4');
#496=NEXT_ASSEMBLY_USAGE_OCCURRENCE('M5x14 Cap Screw:4',
'M5x14 Cap Screw:4','M5x14 Cap Screw:4',#35128,#35162,
'M5x14 Cap Screw:4');
#497=NEXT_ASSEMBLY_USAGE_OCCURRENCE('Captive slot nut:5',
'Captive slot nut:5','Captive slot nut:5',#35128,#35144,
'Captive slot nut:5');
#498=NEXT_ASSEMBLY_USAGE_OCCURRENCE('Flat Washer - M5:5',
'Flat Washer - M5:5','Flat Washer - M5:5',#35128,#35145,
'Flat Washer - M5:5');
#499=NEXT_ASSEMBLY_USAGE_OCCURRENCE('M5x14 Cap Screw:5',
'M5x14 Cap Screw:5','M5x14 Cap Screw:5',#35128,#35162,
'M5x14 Cap Screw:5');
#500=NEXT_ASSEMBLY_USAGE_OCCURRENCE('Captive slot nut:6',
'Captive slot nut:6','Captive slot nut:6',#35128,#35144,
'Captive slot nut:6');
#501=NEXT_ASSEMBLY_USAGE_OCCURRENCE('Flat Washer - M5:6',
'Flat Washer - M5:6','Flat Washer - M5:6',#35128,#35145,
'Flat Washer - M5:6');
#502=NEXT_ASSEMBLY_USAGE_OCCURRENCE('M5x14 Cap Screw:6',
'M5x14 Cap Screw:6','M5x14 Cap Screw:6',#35128,#35162,
'M5x14 Cap Screw:6');
#503=NEXT_ASSEMBLY_USAGE_OCCURRENCE('Captive slot nut:7',
'Captive slot nut:7','Captive slot nut:7',#35128,#35144,
'Captive slot nut:7');
#504=NEXT_ASSEMBLY_USAGE_OCCURRENCE('Flat Washer - M5:7',
'Flat Washer - M5:7','Flat Washer - M5:7',#35128,#35145,
'Flat Washer - M5:7');
#505=NEXT_ASSEMBLY_USAGE_OCCURRENCE('M5x14 Cap Screw:7',
'M5x14 Cap Screw:7','M5x14 Cap Screw:7',#35128,#35162,
'M5x14 Cap Screw:7');
#506=NEXT_ASSEMBLY_USAGE_OCCURRENCE('Captive slot nut:8',
'Captive slot nut:8','Captive slot nut:8',#35128,#35144,
'Captive slot nut:8');
#507=NEXT_ASSEMBLY_USAGE_OCCURRENCE('Flat Washer - M5:8',
'Flat Washer - M5:8','Flat Washer - M5:8',#35128,#35145,
'Flat Washer - M5:8');
#508=NEXT_ASSEMBLY_USAGE_OCCURRENCE('M5x14 Cap Screw:8',
'M5x14 Cap Screw:8','M5x14 Cap Screw:8',#35128,#35162,
'M5x14 Cap Screw:8');
#509=NEXT_ASSEMBLY_USAGE_OCCURRENCE('Captive slot nut:9',
'Captive slot nut:9','Captive slot nut:9',#35128,#35144,
'Captive slot nut:9');
#510=NEXT_ASSEMBLY_USAGE_OCCURRENCE('Flat Washer - M5:9',
'Flat Washer - M5:9','Flat Washer - M5:9',#35128,#35145,
'Flat Washer - M5:9');
#511=NEXT_ASSEMBLY_USAGE_OCCURRENCE('M5x14 Cap Screw:9',
'M5x14 Cap Screw:9','M5x14 Cap Screw:9',#35128,#35162,
'M5x14 Cap Screw:9');
#512=NEXT_ASSEMBLY_USAGE_OCCURRENCE(
'Linear Guide Rail - 15 mm, 220 mm Long:2',
'Linear Guide Rail - 15 mm, 220 mm Long:2',
'Linear Guide Rail - 15 mm, 220 mm Long:2',#35128,#35146,
'Linear Guide Rail - 15 mm, 220 mm Long:2');
#513=NEXT_ASSEMBLY_USAGE_OCCURRENCE('Cap Screw - M4x16:2',
'Cap Screw - M4x16:2','Cap Screw - M4x16:2',#35128,#35174,
'Cap Screw - M4x16:2');
#514=NEXT_ASSEMBLY_USAGE_OCCURRENCE('Cap Screw - M4x16:3',
'Cap Screw - M4x16:3','Cap Screw - M4x16:3',#35128,#35174,
'Cap Screw - M4x16:3');
#515=NEXT_ASSEMBLY_USAGE_OCCURRENCE('Cap Screw - M4x16:4',
'Cap Screw - M4x16:4','Cap Screw - M4x16:4',#35128,#35174,
'Cap Screw - M4x16:4');
#516=NEXT_ASSEMBLY_USAGE_OCCURRENCE('Cap Screw - M4x16:5',
'Cap Screw - M4x16:5','Cap Screw - M4x16:5',#35128,#35174,
'Cap Screw - M4x16:5');
#517=NEXT_ASSEMBLY_USAGE_OCCURRENCE('Cap Screw - M5x20:2',
'Cap Screw - M5x20:2','Cap Screw - M5x20:2',#35128,#35147,
'Cap Screw - M5x20:2');
#518=NEXT_ASSEMBLY_USAGE_OCCURRENCE('Cap Screw - M5x20:3',
'Cap Screw - M5x20:3','Cap Screw - M5x20:3',#35128,#35147,
'Cap Screw - M5x20:3');
#519=NEXT_ASSEMBLY_USAGE_OCCURRENCE('Cap Screw - M5x20:4',
'Cap Screw - M5x20:4','Cap Screw - M5x20:4',#35128,#35147,
'Cap Screw - M5x20:4');
#520=NEXT_ASSEMBLY_USAGE_OCCURRENCE('Cap Screw - M5x20:5',
'Cap Screw - M5x20:5','Cap Screw - M5x20:5',#35128,#35147,
'Cap Screw - M5x20:5');
#521=NEXT_ASSEMBLY_USAGE_OCCURRENCE('Cap Screw - M4x16:10',
'Cap Screw - M4x16:10','Cap Screw - M4x16:10',#35128,#35174,
'Cap Screw - M4x16:10');
#522=NEXT_ASSEMBLY_USAGE_OCCURRENCE('Cap Screw - M4x16:11',
'Cap Screw - M4x16:11','Cap Screw - M4x16:11',#35128,#35174,
'Cap Screw - M4x16:11');
#523=NEXT_ASSEMBLY_USAGE_OCCURRENCE(
'Sealed Ball Bearing - 12 x 32 x 10 mm:2',
'Sealed Ball Bearing - 12 x 32 x 10 mm:2',
'Sealed Ball Bearing - 12 x 32 x 10 mm:2',#35128,#35148,
'Sealed Ball Bearing - 12 x 32 x 10 mm:2');
#524=NEXT_ASSEMBLY_USAGE_OCCURRENCE('M4x10 Cap Screw:2',
'M4x10 Cap Screw:2','M4x10 Cap Screw:2',#35128,#35154,
'M4x10 Cap Screw:2');
#525=NEXT_ASSEMBLY_USAGE_OCCURRENCE('M4x10 Cap Screw:3',
'M4x10 Cap Screw:3','M4x10 Cap Screw:3',#35128,#35154,
'M4x10 Cap Screw:3');
#526=NEXT_ASSEMBLY_USAGE_OCCURRENCE('M4x10 Cap Screw:4',
'M4x10 Cap Screw:4','M4x10 Cap Screw:4',#35128,#35154,
'M4x10 Cap Screw:4');
#527=NEXT_ASSEMBLY_USAGE_OCCURRENCE('M4x10 Cap Screw:5',
'M4x10 Cap Screw:5','M4x10 Cap Screw:5',#35128,#35154,
'M4x10 Cap Screw:5');
#528=NEXT_ASSEMBLY_USAGE_OCCURRENCE('M4x10 Cap Screw:6',
'M4x10 Cap Screw:6','M4x10 Cap Screw:6',#35128,#35154,
'M4x10 Cap Screw:6');
#529=NEXT_ASSEMBLY_USAGE_OCCURRENCE('M4x10 Cap Screw:7',
'M4x10 Cap Screw:7','M4x10 Cap Screw:7',#35128,#35154,
'M4x10 Cap Screw:7');
#530=NEXT_ASSEMBLY_USAGE_OCCURRENCE('M4x10 Cap Screw:8',
'M4x10 Cap Screw:8','M4x10 Cap Screw:8',#35128,#35154,
'M4x10 Cap Screw:8');
#531=NEXT_ASSEMBLY_USAGE_OCCURRENCE('M4x10 Cap Screw:9',
'M4x10 Cap Screw:9','M4x10 Cap Screw:9',#35128,#35154,
'M4x10 Cap Screw:9');
#532=NEXT_ASSEMBLY_USAGE_OCCURRENCE('Cap Screw - M4x16:12',
'Cap Screw - M4x16:12','Cap Screw - M4x16:12',#35128,#35174,
'Cap Screw - M4x16:12');
#533=NEXT_ASSEMBLY_USAGE_OCCURRENCE('Cap Screw - M4x16:13',
'Cap Screw - M4x16:13','Cap Screw - M4x16:13',#35128,#35174,
'Cap Screw - M4x16:13');
#534=NEXT_ASSEMBLY_USAGE_OCCURRENCE(
'Sealed Ball Bearing - 12 x 32 x 10 mm:3',
'Sealed Ball Bearing - 12 x 32 x 10 mm:3',
'Sealed Ball Bearing - 12 x 32 x 10 mm:3',#35128,#35148,
'Sealed Ball Bearing - 12 x 32 x 10 mm:3');
#535=NEXT_ASSEMBLY_USAGE_OCCURRENCE('M4x10 Cap Screw:10',
'M4x10 Cap Screw:10','M4x10 Cap Screw:10',#35128,#35154,
'M4x10 Cap Screw:10');
#536=NEXT_ASSEMBLY_USAGE_OCCURRENCE('M4x10 Cap Screw:11',
'M4x10 Cap Screw:11','M4x10 Cap Screw:11',#35128,#35154,
'M4x10 Cap Screw:11');
#537=NEXT_ASSEMBLY_USAGE_OCCURRENCE('M4x10 Cap Screw:12',
'M4x10 Cap Screw:12','M4x10 Cap Screw:12',#35128,#35154,
'M4x10 Cap Screw:12');
#538=NEXT_ASSEMBLY_USAGE_OCCURRENCE('M4x10 Cap Screw:13',
'M4x10 Cap Screw:13','M4x10 Cap Screw:13',#35128,#35154,
'M4x10 Cap Screw:13');
#539=NEXT_ASSEMBLY_USAGE_OCCURRENCE('M4x10 Cap Screw:14',
'M4x10 Cap Screw:14','M4x10 Cap Screw:14',#35128,#35154,
'M4x10 Cap Screw:14');
#540=NEXT_ASSEMBLY_USAGE_OCCURRENCE('M4x10 Cap Screw:15',
'M4x10 Cap Screw:15','M4x10 Cap Screw:15',#35128,#35154,
'M4x10 Cap Screw:15');
#541=NEXT_ASSEMBLY_USAGE_OCCURRENCE('M4x10 Cap Screw:16',
'M4x10 Cap Screw:16','M4x10 Cap Screw:16',#35128,#35154,
'M4x10 Cap Screw:16');
#542=NEXT_ASSEMBLY_USAGE_OCCURRENCE('M4x10 Cap Screw:17',
'M4x10 Cap Screw:17','M4x10 Cap Screw:17',#35128,#35154,
'M4x10 Cap Screw:17');
#543=NEXT_ASSEMBLY_USAGE_OCCURRENCE('Table:1','Table:1','Table:1',#35155,
#35156,'Table:1');
#544=NEXT_ASSEMBLY_USAGE_OCCURRENCE('Module 2 rack:1','Module 2 rack:1',
'Module 2 rack:1',#35155,#35157,'Module 2 rack:1');
#545=NEXT_ASSEMBLY_USAGE_OCCURRENCE(
'Flanged Linear Guide Carriage - 15 mm:2',
'Flanged Linear Guide Carriage - 15 mm:2',
'Flanged Linear Guide Carriage - 15 mm:2',#35155,#35158,
'Flanged Linear Guide Carriage - 15 mm:2');
#546=NEXT_ASSEMBLY_USAGE_OCCURRENCE('M5x14 Cap Screw:10',
'M5x14 Cap Screw:10','M5x14 Cap Screw:10',#35155,#35162,
'M5x14 Cap Screw:10');
#547=NEXT_ASSEMBLY_USAGE_OCCURRENCE('M5x14 Cap Screw:11',
'M5x14 Cap Screw:11','M5x14 Cap Screw:11',#35155,#35162,
'M5x14 Cap Screw:11');
#548=NEXT_ASSEMBLY_USAGE_OCCURRENCE('M5x14 Cap Screw:12',
'M5x14 Cap Screw:12','M5x14 Cap Screw:12',#35155,#35162,
'M5x14 Cap Screw:12');
#549=NEXT_ASSEMBLY_USAGE_OCCURRENCE('M5x14 Cap Screw:13',
'M5x14 Cap Screw:13','M5x14 Cap Screw:13',#35155,#35162,
'M5x14 Cap Screw:13');
#550=NEXT_ASSEMBLY_USAGE_OCCURRENCE('Cap Screw - M4x16:6',
'Cap Screw - M4x16:6','Cap Screw - M4x16:6',#35155,#35174,
'Cap Screw - M4x16:6');
#551=NEXT_ASSEMBLY_USAGE_OCCURRENCE('Cap Screw - M4x16:7',
'Cap Screw - M4x16:7','Cap Screw - M4x16:7',#35155,#35174,
'Cap Screw - M4x16:7');
#552=NEXT_ASSEMBLY_USAGE_OCCURRENCE('Cap Screw - M4x16:8',
'Cap Screw - M4x16:8','Cap Screw - M4x16:8',#35155,#35174,
'Cap Screw - M4x16:8');
#553=NEXT_ASSEMBLY_USAGE_OCCURRENCE('Cap Screw - M4x16:9',
'Cap Screw - M4x16:9','Cap Screw - M4x16:9',#35155,#35174,
'Cap Screw - M4x16:9');
#554=NEXT_ASSEMBLY_USAGE_OCCURRENCE('Pinion shaft:1','Pinion shaft:1',
'Pinion shaft:1',#35163,#35164,'Pinion shaft:1');
#555=NEXT_ASSEMBLY_USAGE_OCCURRENCE('Gear front spacer:1',
'Gear front spacer:1','Gear front spacer:1',#35163,#35165,
'Gear front spacer:1');
#556=NEXT_ASSEMBLY_USAGE_OCCURRENCE('Rear inner spacer:1',
'Rear inner spacer:1','Rear inner spacer:1',#35163,#35166,
'Rear inner spacer:1');
#557=NEXT_ASSEMBLY_USAGE_OCCURRENCE('Crank inner spacer:1',
'Crank inner spacer:1','Crank inner spacer:1',#35163,#35167,
'Crank inner spacer:1');
#558=NEXT_ASSEMBLY_USAGE_OCCURRENCE('Shaft keeper:1','Shaft keeper:1',
'Shaft keeper:1',#35163,#35168,'Shaft keeper:1');
#559=NEXT_ASSEMBLY_USAGE_OCCURRENCE('Shaft keeper (1):1',
'Shaft keeper (1):1','Shaft keeper (1):1',#35163,#35169,
'Shaft keeper (1):1');
#560=NEXT_ASSEMBLY_USAGE_OCCURRENCE('Rear end sleeve:1',
'Rear end sleeve:1','Rear end sleeve:1',#35163,#35170,
'Rear end sleeve:1');
#561=NEXT_ASSEMBLY_USAGE_OCCURRENCE('Crank:1','Crank:1','Crank:1',#35163,
#35171,'Crank:1');
#562=NEXT_ASSEMBLY_USAGE_OCCURRENCE('Grip bushing:1','Grip bushing:1',
'Grip bushing:1',#35163,#35172,'Grip bushing:1');
#563=NEXT_ASSEMBLY_USAGE_OCCURRENCE(
'Spur Gear - Module 2, 20 Teeth, 12 mm Bore:2',
'Spur Gear - Module 2, 20 Teeth, 12 mm Bore:2',
'Spur Gear - Module 2, 20 Teeth, 12 mm Bore:2',#35163,#35173,
'Spur Gear - Module 2, 20 Teeth, 12 mm Bore:2');
#564=NEXT_ASSEMBLY_USAGE_OCCURRENCE('Key 4x4x14:2','Key 4x4x14:2',
'Key 4x4x14:2',#35163,#35175,'Key 4x4x14:2');
#565=NEXT_ASSEMBLY_USAGE_OCCURRENCE('Cap Screw - M4x16:14',
'Cap Screw - M4x16:14','Cap Screw - M4x16:14',#35163,#35174,
'Cap Screw - M4x16:14');
#566=NEXT_ASSEMBLY_USAGE_OCCURRENCE('Cap Screw - M4x16:15',
'Cap Screw - M4x16:15','Cap Screw - M4x16:15',#35163,#35174,
'Cap Screw - M4x16:15');
#567=NEXT_ASSEMBLY_USAGE_OCCURRENCE('Key 4x4x14:3','Key 4x4x14:3',
'Key 4x4x14:3',#35163,#35175,'Key 4x4x14:3');
#568=NEXT_ASSEMBLY_USAGE_OCCURRENCE('Flat Washer - M6:2',
'Flat Washer - M6:2','Flat Washer - M6:2',#35163,#35176,
'Flat Washer - M6:2');
#569=NEXT_ASSEMBLY_USAGE_OCCURRENCE('Cap Screw - M6x25:2',
'Cap Screw - M6x25:2','Cap Screw - M6x25:2',#35163,#35177,
'Cap Screw - M6x25:2');
#570=NEXT_ASSEMBLY_USAGE_OCCURRENCE('Handle:1','Handle:1','Handle:1',#35178,
#35179,'Handle:1');
#571=NEXT_ASSEMBLY_USAGE_OCCURRENCE(
'Extrusion frame and pinion bearings:1',
'Extrusion frame and pinion bearings:1',
'Extrusion frame and pinion bearings:1',#35127,#35128,
'Extrusion frame and pinion bearings:1');
#572=NEXT_ASSEMBLY_USAGE_OCCURRENCE('Rack and carriage:1',
'Rack and carriage:1','Rack and carriage:1',#35127,#35155,
'Rack and carriage:1');
#573=NEXT_ASSEMBLY_USAGE_OCCURRENCE('Pinion shaft and crank:1',
'Pinion shaft and crank:1','Pinion shaft and crank:1',#35127,#35163,
'Pinion shaft and crank:1');
#574=NEXT_ASSEMBLY_USAGE_OCCURRENCE('Revolving grip:1',
'Revolving grip:1','Revolving grip:1',#35127,#35178,'Revolving grip:1');
#575=B_SPLINE_CURVE_WITH_KNOTS('',3,(#20890,#20891,#20892,#20893,#20894,
#20895,#20896,#20897,#20898,#20899,#20900,#20901,#20902,#20903,#20904,#20905,
#20906,#20907,#20908,#20909,#20910,#20911),.UNSPECIFIED.,.F.,.F.,(4,2,2,
2,2,2,2,2,2,2,4),(0.0591825211272536,0.157966726598481,0.236950089897721,
0.315933453196962,0.391576304923761,0.46721915665056,0.54286200837736,0.618504860104159,
0.697488223403399,0.77647158670264,0.875255792173867),.UNSPECIFIED.);
#576=B_SPLINE_CURVE_WITH_KNOTS('',3,(#20915,#20916,#20917,#20918,#20919,
#20920,#20921,#20922,#20923,#20924,#20925,#20926,#20927,#20928,#20929,#20930,
#20931,#20932,#20933,#20934,#20935,#20936),.UNSPECIFIED.,.F.,.F.,(4,2,2,
2,2,2,2,2,2,2,4),(0.0581119756758434,0.106553146291161,0.213106292582322,
0.30849933801665,0.386091982889075,0.4636846277615,0.541277272633925,0.61886991750635,
0.714262962940678,0.820816109231839,0.869257279847157),.UNSPECIFIED.);
#577=B_SPLINE_CURVE_WITH_KNOTS('',3,(#20942,#20943,#20944,#20945,#20946,
#20947,#20948,#20949,#20950,#20951,#20952,#20953,#20954,#20955,#20956,#20957,
#20958,#20959,#20960,#20961,#20962,#20963),.UNSPECIFIED.,.F.,.F.,(4,2,2,
2,2,2,2,2,2,2,4),(0.0581119756758434,0.106553146291161,0.213106292582322,
0.30849933801665,0.386091982889075,0.4636846277615,0.541277272633925,0.61886991750635,
0.714262962940679,0.820816109231839,0.869257279847157),.UNSPECIFIED.);
#578=B_SPLINE_CURVE_WITH_KNOTS('',3,(#20967,#20968,#20969,#20970,#20971,
#20972,#20973,#20974,#20975,#20976,#20977,#20978,#20979,#20980,#20981,#20982,
#20983,#20984,#20985,#20986,#20987,#20988),.UNSPECIFIED.,.F.,.F.,(4,2,2,
2,2,2,2,2,2,2,4),(0.0581119756758433,0.106553146291161,0.213106292582322,
0.308499338016649,0.386091982889075,0.4636846277615,0.541277272633925,0.61886991750635,
0.714262962940678,0.820816109231839,0.869257279847157),.UNSPECIFIED.);
#579=B_SPLINE_CURVE_WITH_KNOTS('',3,(#20997,#20998,#20999,#21000,#21001,
#21002,#21003,#21004,#21005,#21006,#21007,#21008,#21009,#21010,#21011,#21012,
#21013,#21014,#21015,#21016,#21017,#21018),.UNSPECIFIED.,.F.,.F.,(4,2,2,
2,2,2,2,2,2,2,4),(0.0581119756758433,0.106553146291161,0.213106292582322,
0.30849933801665,0.386091982889075,0.4636846277615,0.541277272633925,0.61886991750635,
0.714262962940678,0.820816109231839,0.869257279847157),.UNSPECIFIED.);
#580=B_SPLINE_CURVE_WITH_KNOTS('',3,(#21022,#21023,#21024,#21025,#21026,
#21027,#21028,#21029,#21030,#21031,#21032,#21033,#21034,#21035,#21036,#21037,
#21038,#21039,#21040,#21041,#21042,#21043),.UNSPECIFIED.,.F.,.F.,(4,2,2,
2,2,2,2,2,2,2,4),(0.0581119756758434,0.106553146291161,0.213106292582322,
0.30849933801665,0.386091982889075,0.4636846277615,0.541277272633925,0.61886991750635,
0.714262962940678,0.820816109231839,0.869257279847157),.UNSPECIFIED.);
#581=B_SPLINE_CURVE_WITH_KNOTS('',3,(#21047,#21048,#21049,#21050,#21051,
#21052,#21053,#21054,#21055,#21056,#21057,#21058,#21059,#21060,#21061,#21062,
#21063,#21064,#21065,#21066,#21067,#21068),.UNSPECIFIED.,.F.,.F.,(4,2,2,
2,2,2,2,2,2,2,4),(0.0581119756758434,0.106553146291161,0.213106292582322,
0.30849933801665,0.386091982889075,0.4636846277615,0.541277272633925,0.61886991750635,
0.714262962940678,0.820816109231839,0.869257279847157),.UNSPECIFIED.);
#582=B_SPLINE_CURVE_WITH_KNOTS('',3,(#21072,#21073,#21074,#21075,#21076,
#21077,#21078,#21079,#21080,#21081,#21082,#21083,#21084,#21085,#21086,#21087,
#21088,#21089,#21090,#21091,#21092,#21093),.UNSPECIFIED.,.F.,.F.,(4,2,2,
2,2,2,2,2,2,2,4),(0.0581119756758433,0.106553146291161,0.213106292582322,
0.30849933801665,0.386091982889075,0.4636846277615,0.541277272633925,0.61886991750635,
0.714262962940678,0.820816109231839,0.869257279847157),.UNSPECIFIED.);
#583=B_SPLINE_CURVE_WITH_KNOTS('',3,(#21101,#21102,#21103,#21104,#21105,
#21106,#21107,#21108,#21109,#21110,#21111,#21112,#21113,#21114,#21115,#21116,
#21117,#21118,#21119,#21120,#21121,#21122),.UNSPECIFIED.,.F.,.F.,(4,2,2,
2,2,2,2,2,2,2,4),(0.0591825211272536,0.157966726598481,0.236950089897721,
0.315933453196962,0.391576304923761,0.467219156650561,0.54286200837736,
0.618504860104159,0.697488223403399,0.77647158670264,0.875255792173867),
 .UNSPECIFIED.);
#584=B_SPLINE_CURVE_WITH_KNOTS('',3,(#21130,#21131,#21132,#21133,#21134,
#21135,#21136,#21137,#21138,#21139,#21140,#21141,#21142,#21143,#21144,#21145,
#21146,#21147,#21148,#21149,#21150,#21151),.UNSPECIFIED.,.F.,.F.,(4,2,2,
2,2,2,2,2,2,2,4),(0.0591825211272536,0.157966726598481,0.236950089897722,
0.315933453196962,0.391576304923761,0.467219156650561,0.54286200837736,
0.618504860104159,0.697488223403399,0.77647158670264,0.875255792173867),
 .UNSPECIFIED.);
#585=B_SPLINE_CURVE_WITH_KNOTS('',3,(#21161,#21162,#21163,#21164,#21165,
#21166,#21167,#21168,#21169,#21170,#21171,#21172,#21173,#21174,#21175,#21176,
#21177,#21178,#21179,#21180,#21181,#21182),.UNSPECIFIED.,.F.,.F.,(4,2,2,
2,2,2,2,2,2,2,4),(0.0591825211272536,0.157966726598481,0.236950089897721,
0.315933453196962,0.391576304923761,0.46721915665056,0.54286200837736,0.618504860104159,
0.697488223403399,0.77647158670264,0.875255792173867),.UNSPECIFIED.);
#586=B_SPLINE_CURVE_WITH_KNOTS('',3,(#21190,#21191,#21192,#21193,#21194,
#21195,#21196,#21197,#21198,#21199,#21200,#21201,#21202,#21203,#21204,#21205,
#21206,#21207,#21208,#21209,#21210,#21211),.UNSPECIFIED.,.F.,.F.,(4,2,2,
2,2,2,2,2,2,2,4),(0.0591825211272536,0.157966726598481,0.236950089897721,
0.315933453196962,0.391576304923761,0.46721915665056,0.542862008377359,
0.618504860104159,0.697488223403399,0.776471586702639,0.875255792173867),
 .UNSPECIFIED.);
#587=B_SPLINE_CURVE_WITH_KNOTS('',3,(#21219,#21220,#21221,#21222,#21223,
#21224,#21225,#21226,#21227,#21228,#21229,#21230,#21231,#21232,#21233,#21234,
#21235,#21236,#21237,#21238,#21239,#21240),.UNSPECIFIED.,.F.,.F.,(4,2,2,
2,2,2,2,2,2,2,4),(0.0591825211272536,0.157966726598481,0.236950089897721,
0.315933453196962,0.391576304923761,0.46721915665056,0.54286200837736,0.618504860104159,
0.697488223403399,0.77647158670264,0.875255792173867),.UNSPECIFIED.);
#588=B_SPLINE_CURVE_WITH_KNOTS('',3,(#21249,#21250,#21251,#21252,#21253,
#21254,#21255,#21256,#21257,#21258,#21259,#21260,#21261,#21262,#21263,#21264,
#21265,#21266,#21267,#21268,#21269,#21270),.UNSPECIFIED.,.F.,.F.,(4,2,2,
2,2,2,2,2,2,2,4),(0.0591825211272536,0.157966726598481,0.236950089897721,
0.315933453196962,0.391576304923761,0.46721915665056,0.542862008377359,
0.618504860104159,0.697488223403399,0.776471586702639,0.875255792173867),
 .UNSPECIFIED.);
#589=SPHERICAL_SURFACE('',#14820,0.29765);
#590=SPHERICAL_SURFACE('',#14822,0.29765);
#591=SPHERICAL_SURFACE('',#14824,0.29765);
#592=SPHERICAL_SURFACE('',#14826,0.29765);
#593=SPHERICAL_SURFACE('',#14828,0.29765);
#594=SPHERICAL_SURFACE('',#14830,0.29765);
#595=SPHERICAL_SURFACE('',#14832,0.29765);
#596=SPHERICAL_SURFACE('',#14835,0.309556);
#597=SPHERICAL_SURFACE('',#14851,0.309556);
#598=SPHERICAL_SURFACE('',#14856,0.309556);
#599=SPHERICAL_SURFACE('',#14862,0.309556);
#600=SPHERICAL_SURFACE('',#14867,0.309556);
#601=SPHERICAL_SURFACE('',#14872,0.309556);
#602=SPHERICAL_SURFACE('',#14880,0.309556);
#603=TOROIDAL_SURFACE('',#14780,1.1,0.309556);
#604=TOROIDAL_SURFACE('',#14800,1.1,0.309556);
#605=ORIENTED_CLOSED_SHELL('',*,#13771,.F.);
#606=ORIENTED_CLOSED_SHELL('',*,#13784,.F.);
#607=ORIENTED_CLOSED_SHELL('',*,#13791,.F.);
#608=ORIENTED_CLOSED_SHELL('',*,#13804,.F.);
#609=ORIENTED_CLOSED_SHELL('',*,#13808,.F.);
#610=BREP_WITH_VOIDS('Body1',#13770,(#605));
#611=BREP_WITH_VOIDS('Body1',#13785,(#606));
#612=BREP_WITH_VOIDS('Body1',#13792,(#607));
#613=BREP_WITH_VOIDS('Body1',#13803,(#608));
#614=BREP_WITH_VOIDS('Body1',#13807,(#609));
#615=CONICAL_SURFACE('',#14699,0.275,0.785398163397449);
#616=CONICAL_SURFACE('',#14755,0.4,0.785398163397448);
#617=CONICAL_SURFACE('',#14759,0.41,0.785398163397448);
#618=CONICAL_SURFACE('',#14763,0.26,0.463647609000806);
#619=CONICAL_SURFACE('',#14767,0.225,0.785398163397448);
#620=CONICAL_SURFACE('',#14791,0.63,0.785398163397448);
#621=CONICAL_SURFACE('',#14798,0.63,0.785398163397448);
#622=CONICAL_SURFACE('',#14811,1.57,0.785398163397449);
#623=CONICAL_SURFACE('',#14815,1.57,0.785398163397449);
#624=CONICAL_SURFACE('',#14919,0.325,0.785398163397448);
#625=CONICAL_SURFACE('',#14923,0.335,0.785398163397448);
#626=CONICAL_SURFACE('',#14927,0.21,0.463647609000806);
#627=CONICAL_SURFACE('',#15187,0.4,0.785398163397448);
#628=CONICAL_SURFACE('',#15191,0.41,0.785398163397448);
#629=CONICAL_SURFACE('',#15195,0.26,0.463647609000806);
#630=CONICAL_SURFACE('',#15418,0.325,0.785398163397448);
#631=CONICAL_SURFACE('',#15422,0.335,0.785398163397448);
#632=CONICAL_SURFACE('',#15426,0.21,0.463647609000806);
#633=CONICAL_SURFACE('',#15430,0.18,0.785398163397448);
#634=CONICAL_SURFACE('',#15546,0.475,0.785398163397449);
#635=CONICAL_SURFACE('',#15550,0.485,0.785398163397448);
#636=CONICAL_SURFACE('',#15554,0.31,0.463647609000806);
#637=CONICAL_SURFACE('',#15558,0.27,0.785398163397448);
#638=ELLIPSE('',#14688,0.299389011154384,0.2117);
#639=ELLIPSE('',#14692,0.299389011154384,0.2117);
#640=SHAPE_REPRESENTATION_RELATIONSHIP('SRR','None',#35075,#686);
#641=SHAPE_REPRESENTATION_RELATIONSHIP('SRR','None',#35076,#687);
#642=SHAPE_REPRESENTATION_RELATIONSHIP('SRR','None',#35077,#688);
#643=SHAPE_REPRESENTATION_RELATIONSHIP('SRR','None',#35078,#689);
#644=SHAPE_REPRESENTATION_RELATIONSHIP('SRR','None',#35079,#690);
#645=SHAPE_REPRESENTATION_RELATIONSHIP('SRR','None',#35080,#691);
#646=SHAPE_REPRESENTATION_RELATIONSHIP('SRR','None',#35081,#692);
#647=SHAPE_REPRESENTATION_RELATIONSHIP('SRR','None',#35082,#693);
#648=SHAPE_REPRESENTATION_RELATIONSHIP('SRR','None',#35083,#694);
#649=SHAPE_REPRESENTATION_RELATIONSHIP('SRR','None',#35084,#695);
#650=SHAPE_REPRESENTATION_RELATIONSHIP('SRR','None',#35085,#696);
#651=SHAPE_REPRESENTATION_RELATIONSHIP('SRR','None',#35086,#697);
#652=SHAPE_REPRESENTATION_RELATIONSHIP('SRR','None',#35087,#698);
#653=SHAPE_REPRESENTATION_RELATIONSHIP('SRR','None',#35088,#699);
#654=SHAPE_REPRESENTATION_RELATIONSHIP('SRR','None',#35089,#700);
#655=SHAPE_REPRESENTATION_RELATIONSHIP('SRR','None',#35090,#701);
#656=SHAPE_REPRESENTATION_RELATIONSHIP('SRR','None',#35091,#702);
#657=SHAPE_REPRESENTATION_RELATIONSHIP('SRR','None',#35092,#703);
#658=SHAPE_REPRESENTATION_RELATIONSHIP('SRR','None',#35093,#704);
#659=SHAPE_REPRESENTATION_RELATIONSHIP('SRR','None',#35095,#705);
#660=SHAPE_REPRESENTATION_RELATIONSHIP('SRR','None',#35096,#706);
#661=SHAPE_REPRESENTATION_RELATIONSHIP('SRR','None',#35097,#707);
#662=SHAPE_REPRESENTATION_RELATIONSHIP('SRR','None',#35098,#708);
#663=SHAPE_REPRESENTATION_RELATIONSHIP('SRR','None',#35099,#709);
#664=SHAPE_REPRESENTATION_RELATIONSHIP('SRR','None',#35100,#710);
#665=SHAPE_REPRESENTATION_RELATIONSHIP('SRR','None',#35102,#711);
#666=SHAPE_REPRESENTATION_RELATIONSHIP('SRR','None',#35103,#712);
#667=SHAPE_REPRESENTATION_RELATIONSHIP('SRR','None',#35105,#713);
#668=SHAPE_REPRESENTATION_RELATIONSHIP('SRR','None',#35106,#714);
#669=SHAPE_REPRESENTATION_RELATIONSHIP('SRR','None',#35107,#715);
#670=SHAPE_REPRESENTATION_RELATIONSHIP('SRR','None',#35108,#716);
#671=SHAPE_REPRESENTATION_RELATIONSHIP('SRR','None',#35110,#717);
#672=SHAPE_REPRESENTATION_RELATIONSHIP('SRR','None',#35111,#718);
#673=SHAPE_REPRESENTATION_RELATIONSHIP('SRR','None',#35112,#719);
#674=SHAPE_REPRESENTATION_RELATIONSHIP('SRR','None',#35113,#720);
#675=SHAPE_REPRESENTATION_RELATIONSHIP('SRR','None',#35114,#721);
#676=SHAPE_REPRESENTATION_RELATIONSHIP('SRR','None',#35115,#722);
#677=SHAPE_REPRESENTATION_RELATIONSHIP('SRR','None',#35116,#723);
#678=SHAPE_REPRESENTATION_RELATIONSHIP('SRR','None',#35117,#724);
#679=SHAPE_REPRESENTATION_RELATIONSHIP('SRR','None',#35118,#725);
#680=SHAPE_REPRESENTATION_RELATIONSHIP('SRR','None',#35119,#726);
#681=SHAPE_REPRESENTATION_RELATIONSHIP('SRR','None',#35120,#727);
#682=SHAPE_REPRESENTATION_RELATIONSHIP('SRR','None',#35121,#728);
#683=SHAPE_REPRESENTATION_RELATIONSHIP('SRR','None',#35122,#729);
#684=SHAPE_REPRESENTATION_RELATIONSHIP('SRR','None',#35123,#730);
#685=SHAPE_REPRESENTATION_RELATIONSHIP('SRR','None',#35125,#731);
#686=ADVANCED_BREP_SHAPE_REPRESENTATION('',(#785),#34800);
#687=ADVANCED_BREP_SHAPE_REPRESENTATION('',(#786),#34801);
#688=ADVANCED_BREP_SHAPE_REPRESENTATION('',(#787),#34802);
#689=ADVANCED_BREP_SHAPE_REPRESENTATION('',(#788),#34803);
#690=ADVANCED_BREP_SHAPE_REPRESENTATION('',(#789),#34804);
#691=ADVANCED_BREP_SHAPE_REPRESENTATION('',(#790),#34805);
#692=ADVANCED_BREP_SHAPE_REPRESENTATION('',(#791),#34806);
#693=ADVANCED_BREP_SHAPE_REPRESENTATION('',(#792),#34807);
#694=ADVANCED_BREP_SHAPE_REPRESENTATION('',(#793),#34808);
#695=ADVANCED_BREP_SHAPE_REPRESENTATION('',(#794),#34809);
#696=ADVANCED_BREP_SHAPE_REPRESENTATION('',(#795),#34810);
#697=ADVANCED_BREP_SHAPE_REPRESENTATION('',(#796),#34811);
#698=ADVANCED_BREP_SHAPE_REPRESENTATION('',(#797),#34812);
#699=ADVANCED_BREP_SHAPE_REPRESENTATION('',(#798),#34813);
#700=ADVANCED_BREP_SHAPE_REPRESENTATION('',(#799),#34814);
#701=ADVANCED_BREP_SHAPE_REPRESENTATION('',(#800),#34815);
#702=ADVANCED_BREP_SHAPE_REPRESENTATION('',(#801),#34816);
#703=ADVANCED_BREP_SHAPE_REPRESENTATION('',(#802),#34817);
#704=ADVANCED_BREP_SHAPE_REPRESENTATION('',(#610),#34818);
#705=ADVANCED_BREP_SHAPE_REPRESENTATION('',(#803),#34820);
#706=ADVANCED_BREP_SHAPE_REPRESENTATION('',(#804),#34821);
#707=ADVANCED_BREP_SHAPE_REPRESENTATION('',(#805,#806,#807,#808,#809,#810,
#811),#34822);
#708=ADVANCED_BREP_SHAPE_REPRESENTATION('',(#812),#34823);
#709=ADVANCED_BREP_SHAPE_REPRESENTATION('',(#813,#814),#34824);
#710=ADVANCED_BREP_SHAPE_REPRESENTATION('',(#611),#34825);
#711=ADVANCED_BREP_SHAPE_REPRESENTATION('',(#815),#34827);
#712=ADVANCED_BREP_SHAPE_REPRESENTATION('',(#816),#34828);
#713=ADVANCED_BREP_SHAPE_REPRESENTATION('',(#817),#34830);
#714=ADVANCED_BREP_SHAPE_REPRESENTATION('',(#818),#34831);
#715=ADVANCED_BREP_SHAPE_REPRESENTATION('',(#819),#34832);
#716=ADVANCED_BREP_SHAPE_REPRESENTATION('',(#612),#34833);
#717=ADVANCED_BREP_SHAPE_REPRESENTATION('',(#820),#34835);
#718=ADVANCED_BREP_SHAPE_REPRESENTATION('',(#821),#34836);
#719=ADVANCED_BREP_SHAPE_REPRESENTATION('',(#822),#34837);
#720=ADVANCED_BREP_SHAPE_REPRESENTATION('',(#823),#34838);
#721=ADVANCED_BREP_SHAPE_REPRESENTATION('',(#824),#34839);
#722=ADVANCED_BREP_SHAPE_REPRESENTATION('',(#825),#34840);
#723=ADVANCED_BREP_SHAPE_REPRESENTATION('',(#826),#34841);
#724=ADVANCED_BREP_SHAPE_REPRESENTATION('',(#827),#34842);
#725=ADVANCED_BREP_SHAPE_REPRESENTATION('',(#828),#34843);
#726=ADVANCED_BREP_SHAPE_REPRESENTATION('',(#829),#34844);
#727=ADVANCED_BREP_SHAPE_REPRESENTATION('',(#613),#34845);
#728=ADVANCED_BREP_SHAPE_REPRESENTATION('',(#830),#34846);
#729=ADVANCED_BREP_SHAPE_REPRESENTATION('',(#831),#34847);
#730=ADVANCED_BREP_SHAPE_REPRESENTATION('',(#614),#34848);
#731=ADVANCED_BREP_SHAPE_REPRESENTATION('',(#832),#34850);
#732=STYLED_ITEM('',(#35390),#785);
#733=STYLED_ITEM('',(#35397),#786);
#734=STYLED_ITEM('',(#35397),#787);
#735=STYLED_ITEM('',(#35425),#788);
#736=STYLED_ITEM('',(#35404),#789);
#737=STYLED_ITEM('',(#35404),#790);
#738=STYLED_ITEM('',(#35404),#791);
#739=STYLED_ITEM('',(#35404),#792);
#740=STYLED_ITEM('',(#35411),#793);
#741=STYLED_ITEM('',(#35411),#794);
#742=STYLED_ITEM('',(#35411),#795);
#743=STYLED_ITEM('',(#35411),#796);
#744=STYLED_ITEM('',(#35411),#797);
#745=STYLED_ITEM('',(#35411),#798);
#746=STYLED_ITEM('',(#35425),#799);
#747=STYLED_ITEM('',(#35418),#800);
#748=STYLED_ITEM('',(#35418),#801);
#749=STYLED_ITEM('',(#35404),#802);
#750=STYLED_ITEM('',(#35418),#610);
#751=STYLED_ITEM('',(#35411),#803);
#752=STYLED_ITEM('',(#35411),#804);
#753=STYLED_ITEM('',(#35411),#805);
#754=STYLED_ITEM('',(#35411),#806);
#755=STYLED_ITEM('',(#35411),#807);
#756=STYLED_ITEM('',(#35411),#808);
#757=STYLED_ITEM('',(#35411),#809);
#758=STYLED_ITEM('',(#35411),#810);
#759=STYLED_ITEM('',(#35411),#811);
#760=STYLED_ITEM('',(#35411),#812);
#761=STYLED_ITEM('',(#35411),#813);
#762=STYLED_ITEM('',(#35411),#814);
#763=STYLED_ITEM('',(#35418),#611);
#764=STYLED_ITEM('',(#35425),#815);
#765=STYLED_ITEM('',(#35397),#816);
#766=STYLED_ITEM('',(#35390),#817);
#767=STYLED_ITEM('',(#35404),#818);
#768=STYLED_ITEM('',(#35425),#819);
#769=STYLED_ITEM('',(#35418),#612);
#770=STYLED_ITEM('',(#35411),#820);
#771=STYLED_ITEM('',(#35404),#821);
#772=STYLED_ITEM('',(#35404),#822);
#773=STYLED_ITEM('',(#35404),#823);
#774=STYLED_ITEM('',(#35411),#824);
#775=STYLED_ITEM('',(#35411),#825);
#776=STYLED_ITEM('',(#35404),#826);
#777=STYLED_ITEM('',(#35425),#827);
#778=STYLED_ITEM('',(#35418),#828);
#779=STYLED_ITEM('',(#35425),#829);
#780=STYLED_ITEM('',(#35418),#613);
#781=STYLED_ITEM('',(#35411),#830);
#782=STYLED_ITEM('',(#35418),#831);
#783=STYLED_ITEM('',(#35418),#614);
#784=STYLED_ITEM('',(#35404),#832);
#785=MANIFOLD_SOLID_BREP('Body1',#13752);
#786=MANIFOLD_SOLID_BREP('Body1',#13753);
#787=MANIFOLD_SOLID_BREP('Body1',#13754);
#788=MANIFOLD_SOLID_BREP('Body1',#13755);
#789=MANIFOLD_SOLID_BREP('Body1',#13756);
#790=MANIFOLD_SOLID_BREP('Body1',#13757);
#791=MANIFOLD_SOLID_BREP('Body1',#13758);
#792=MANIFOLD_SOLID_BREP('Body1',#13759);
#793=MANIFOLD_SOLID_BREP('Body1',#13760);
#794=MANIFOLD_SOLID_BREP('Body1',#13761);
#795=MANIFOLD_SOLID_BREP('Body1',#13762);
#796=MANIFOLD_SOLID_BREP('Body1',#13763);
#797=MANIFOLD_SOLID_BREP('Body1',#13764);
#798=MANIFOLD_SOLID_BREP('Body1',#13765);
#799=MANIFOLD_SOLID_BREP('Body1',#13766);
#800=MANIFOLD_SOLID_BREP('Body1',#13767);
#801=MANIFOLD_SOLID_BREP('Body1',#13768);
#802=MANIFOLD_SOLID_BREP('Body1',#13769);
#803=MANIFOLD_SOLID_BREP('Body1',#13772);
#804=MANIFOLD_SOLID_BREP('Body1',#13773);
#805=MANIFOLD_SOLID_BREP('Body1',#13774);
#806=MANIFOLD_SOLID_BREP('Body2',#13775);
#807=MANIFOLD_SOLID_BREP('Body3',#13776);
#808=MANIFOLD_SOLID_BREP('Body4',#13777);
#809=MANIFOLD_SOLID_BREP('Body5',#13778);
#810=MANIFOLD_SOLID_BREP('Body6',#13779);
#811=MANIFOLD_SOLID_BREP('Body7',#13780);
#812=MANIFOLD_SOLID_BREP('Continuous crown cage',#13781);
#813=MANIFOLD_SOLID_BREP('Body1',#13782);
#814=MANIFOLD_SOLID_BREP('Body2',#13783);
#815=MANIFOLD_SOLID_BREP('Body1',#13786);
#816=MANIFOLD_SOLID_BREP('Body1',#13787);
#817=MANIFOLD_SOLID_BREP('Body1',#13788);
#818=MANIFOLD_SOLID_BREP('Body1',#13789);
#819=MANIFOLD_SOLID_BREP('Body1',#13790);
#820=MANIFOLD_SOLID_BREP('Body1',#13793);
#821=MANIFOLD_SOLID_BREP('Body1',#13794);
#822=MANIFOLD_SOLID_BREP('Body1',#13795);
#823=MANIFOLD_SOLID_BREP('Body1',#13796);
#824=MANIFOLD_SOLID_BREP('Body1',#13797);
#825=MANIFOLD_SOLID_BREP('Body1',#13798);
#826=MANIFOLD_SOLID_BREP('Body1',#13799);
#827=MANIFOLD_SOLID_BREP('Body1',#13800);
#828=MANIFOLD_SOLID_BREP('Body1',#13801);
#829=MANIFOLD_SOLID_BREP('Body1',#13802);
#830=MANIFOLD_SOLID_BREP('Body1',#13805);
#831=MANIFOLD_SOLID_BREP('Body1',#13806);
#832=MANIFOLD_SOLID_BREP('Body1',#13809);
#833=FACE_BOUND('',#2283,.T.);
#834=FACE_BOUND('',#2284,.T.);
#835=FACE_BOUND('',#2285,.T.);
#836=FACE_BOUND('',#2286,.T.);
#837=FACE_BOUND('',#2288,.T.);
#838=FACE_BOUND('',#2289,.T.);
#839=FACE_BOUND('',#2290,.T.);
#840=FACE_BOUND('',#2291,.T.);
#841=FACE_BOUND('',#2325,.T.);
#842=FACE_BOUND('',#2326,.T.);
#843=FACE_BOUND('',#2327,.T.);
#844=FACE_BOUND('',#2328,.T.);
#845=FACE_BOUND('',#2329,.T.);
#846=FACE_BOUND('',#2330,.T.);
#847=FACE_BOUND('',#2331,.T.);
#848=FACE_BOUND('',#2332,.T.);
#849=FACE_BOUND('',#2333,.T.);
#850=FACE_BOUND('',#2334,.T.);
#851=FACE_BOUND('',#2335,.T.);
#852=FACE_BOUND('',#2336,.T.);
#853=FACE_BOUND('',#2337,.T.);
#854=FACE_BOUND('',#2338,.T.);
#855=FACE_BOUND('',#2339,.T.);
#856=FACE_BOUND('',#2340,.T.);
#857=FACE_BOUND('',#2342,.T.);
#858=FACE_BOUND('',#2343,.T.);
#859=FACE_BOUND('',#2344,.T.);
#860=FACE_BOUND('',#2345,.T.);
#861=FACE_BOUND('',#2346,.T.);
#862=FACE_BOUND('',#2347,.T.);
#863=FACE_BOUND('',#2348,.T.);
#864=FACE_BOUND('',#2349,.T.);
#865=FACE_BOUND('',#2350,.T.);
#866=FACE_BOUND('',#2351,.T.);
#867=FACE_BOUND('',#2352,.T.);
#868=FACE_BOUND('',#2353,.T.);
#869=FACE_BOUND('',#2354,.T.);
#870=FACE_BOUND('',#2355,.T.);
#871=FACE_BOUND('',#2356,.T.);
#872=FACE_BOUND('',#2357,.T.);
#873=FACE_BOUND('',#2360,.T.);
#874=FACE_BOUND('',#2363,.T.);
#875=FACE_BOUND('',#2371,.T.);
#876=FACE_BOUND('',#2372,.T.);
#877=FACE_BOUND('',#2374,.T.);
#878=FACE_BOUND('',#2375,.T.);
#879=FACE_BOUND('',#2384,.T.);
#880=FACE_BOUND('',#2387,.T.);
#881=FACE_BOUND('',#2395,.T.);
#882=FACE_BOUND('',#2396,.T.);
#883=FACE_BOUND('',#2398,.T.);
#884=FACE_BOUND('',#2399,.T.);
#885=FACE_BOUND('',#2414,.T.);
#886=FACE_BOUND('',#2416,.T.);
#887=FACE_BOUND('',#2420,.T.);
#888=FACE_BOUND('',#2421,.T.);
#889=FACE_BOUND('',#2422,.T.);
#890=FACE_BOUND('',#2423,.T.);
#891=FACE_BOUND('',#2424,.T.);
#892=FACE_BOUND('',#2427,.T.);
#893=FACE_BOUND('',#2428,.T.);
#894=FACE_BOUND('',#2429,.T.);
#895=FACE_BOUND('',#2430,.T.);
#896=FACE_BOUND('',#2431,.T.);
#897=FACE_BOUND('',#2435,.T.);
#898=FACE_BOUND('',#2436,.T.);
#899=FACE_BOUND('',#2443,.T.);
#900=FACE_BOUND('',#2447,.T.);
#901=FACE_BOUND('',#2448,.T.);
#902=FACE_BOUND('',#2449,.T.);
#903=FACE_BOUND('',#2450,.T.);
#904=FACE_BOUND('',#2451,.T.);
#905=FACE_BOUND('',#2453,.T.);
#906=FACE_BOUND('',#2454,.T.);
#907=FACE_BOUND('',#2455,.T.);
#908=FACE_BOUND('',#2456,.T.);
#909=FACE_BOUND('',#2457,.T.);
#910=FACE_BOUND('',#2464,.T.);
#911=FACE_BOUND('',#2468,.T.);
#912=FACE_BOUND('',#2469,.T.);
#913=FACE_BOUND('',#2470,.T.);
#914=FACE_BOUND('',#2471,.T.);
#915=FACE_BOUND('',#2472,.T.);
#916=FACE_BOUND('',#2474,.T.);
#917=FACE_BOUND('',#2475,.T.);
#918=FACE_BOUND('',#2476,.T.);
#919=FACE_BOUND('',#2477,.T.);
#920=FACE_BOUND('',#2478,.T.);
#921=FACE_BOUND('',#2487,.T.);
#922=FACE_BOUND('',#2489,.T.);
#923=FACE_BOUND('',#2493,.T.);
#924=FACE_BOUND('',#2494,.T.);
#925=FACE_BOUND('',#2495,.T.);
#926=FACE_BOUND('',#2496,.T.);
#927=FACE_BOUND('',#2497,.T.);
#928=FACE_BOUND('',#2500,.T.);
#929=FACE_BOUND('',#2501,.T.);
#930=FACE_BOUND('',#2502,.T.);
#931=FACE_BOUND('',#2503,.T.);
#932=FACE_BOUND('',#2504,.T.);
#933=FACE_BOUND('',#2508,.T.);
#934=FACE_BOUND('',#2509,.T.);
#935=FACE_BOUND('',#2516,.T.);
#936=FACE_BOUND('',#2520,.T.);
#937=FACE_BOUND('',#2521,.T.);
#938=FACE_BOUND('',#2522,.T.);
#939=FACE_BOUND('',#2523,.T.);
#940=FACE_BOUND('',#2524,.T.);
#941=FACE_BOUND('',#2526,.T.);
#942=FACE_BOUND('',#2527,.T.);
#943=FACE_BOUND('',#2528,.T.);
#944=FACE_BOUND('',#2529,.T.);
#945=FACE_BOUND('',#2530,.T.);
#946=FACE_BOUND('',#2537,.T.);
#947=FACE_BOUND('',#2541,.T.);
#948=FACE_BOUND('',#2542,.T.);
#949=FACE_BOUND('',#2543,.T.);
#950=FACE_BOUND('',#2544,.T.);
#951=FACE_BOUND('',#2545,.T.);
#952=FACE_BOUND('',#2547,.T.);
#953=FACE_BOUND('',#2548,.T.);
#954=FACE_BOUND('',#2549,.T.);
#955=FACE_BOUND('',#2550,.T.);
#956=FACE_BOUND('',#2551,.T.);
#957=FACE_BOUND('',#2598,.T.);
#958=FACE_BOUND('',#2600,.T.);
#959=FACE_BOUND('',#2604,.T.);
#960=FACE_BOUND('',#2619,.T.);
#961=FACE_BOUND('',#2622,.T.);
#962=FACE_BOUND('',#2625,.T.);
#963=FACE_BOUND('',#2628,.T.);
#964=FACE_BOUND('',#2631,.T.);
#965=FACE_BOUND('',#2634,.T.);
#966=FACE_BOUND('',#2644,.T.);
#967=FACE_BOUND('',#2645,.T.);
#968=FACE_BOUND('',#2646,.T.);
#969=FACE_BOUND('',#2647,.T.);
#970=FACE_BOUND('',#2654,.T.);
#971=FACE_BOUND('',#2655,.T.);
#972=FACE_BOUND('',#2656,.T.);
#973=FACE_BOUND('',#2657,.T.);
#974=FACE_BOUND('',#2666,.T.);
#975=FACE_BOUND('',#2684,.T.);
#976=FACE_BOUND('',#2687,.T.);
#977=FACE_BOUND('',#2692,.T.);
#978=FACE_BOUND('',#2697,.T.);
#979=FACE_BOUND('',#2722,.T.);
#980=FACE_BOUND('',#2725,.T.);
#981=FACE_BOUND('',#2728,.T.);
#982=FACE_BOUND('',#2731,.T.);
#983=FACE_BOUND('',#2734,.T.);
#984=FACE_BOUND('',#2750,.T.);
#985=FACE_BOUND('',#2766,.T.);
#986=FACE_BOUND('',#2767,.T.);
#987=FACE_BOUND('',#2768,.T.);
#988=FACE_BOUND('',#2769,.T.);
#989=FACE_BOUND('',#2770,.T.);
#990=FACE_BOUND('',#2771,.T.);
#991=FACE_BOUND('',#2772,.T.);
#992=FACE_BOUND('',#2773,.T.);
#993=FACE_BOUND('',#2775,.T.);
#994=FACE_BOUND('',#2776,.T.);
#995=FACE_BOUND('',#2777,.T.);
#996=FACE_BOUND('',#2778,.T.);
#997=FACE_BOUND('',#2779,.T.);
#998=FACE_BOUND('',#2780,.T.);
#999=FACE_BOUND('',#2781,.T.);
#1000=FACE_BOUND('',#2782,.T.);
#1001=FACE_BOUND('',#2793,.T.);
#1002=FACE_BOUND('',#2794,.T.);
#1003=FACE_BOUND('',#2795,.T.);
#1004=FACE_BOUND('',#2796,.T.);
#1005=FACE_BOUND('',#2939,.T.);
#1006=FACE_BOUND('',#2940,.T.);
#1007=FACE_BOUND('',#2941,.T.);
#1008=FACE_BOUND('',#2942,.T.);
#1009=FACE_BOUND('',#2985,.T.);
#1010=FACE_BOUND('',#3003,.T.);
#1011=FACE_BOUND('',#3005,.T.);
#1012=FACE_BOUND('',#3009,.T.);
#1013=FACE_BOUND('',#3010,.T.);
#1014=FACE_BOUND('',#3012,.T.);
#1015=FACE_BOUND('',#3014,.T.);
#1016=FACE_BOUND('',#3018,.T.);
#1017=FACE_BOUND('',#3020,.T.);
#1018=FACE_BOUND('',#3024,.T.);
#1019=FACE_BOUND('',#3026,.T.);
#1020=FACE_BOUND('',#3030,.T.);
#1021=FACE_BOUND('',#3032,.T.);
#1022=FACE_BOUND('',#3036,.T.);
#1023=FACE_BOUND('',#3038,.T.);
#1024=FACE_BOUND('',#3042,.T.);
#1025=FACE_BOUND('',#3044,.T.);
#1026=FACE_BOUND('',#3048,.T.);
#1027=FACE_BOUND('',#3050,.T.);
#1028=FACE_BOUND('',#3056,.T.);
#1029=FACE_BOUND('',#3061,.T.);
#1030=FACE_BOUND('',#3064,.T.);
#1031=FACE_BOUND('',#3066,.T.);
#1032=FACE_BOUND('',#3068,.T.);
#1033=FACE_BOUND('',#3072,.T.);
#1034=FACE_BOUND('',#3074,.T.);
#1035=FACE_BOUND('',#3079,.T.);
#1036=FACE_BOUND('',#3083,.T.);
#1037=FACE_BOUND('',#3164,.T.);
#1038=FACE_BOUND('',#3171,.T.);
#1039=FACE_BOUND('',#3197,.T.);
#1040=FACE_BOUND('',#3199,.T.);
#1041=FACE_BOUND('',#3205,.T.);
#1042=FACE_BOUND('',#3221,.T.);
#1043=FACE_BOUND('',#3223,.T.);
#1044=PLANE('',#14332);
#1045=PLANE('',#14333);
#1046=PLANE('',#14334);
#1047=PLANE('',#14335);
#1048=PLANE('',#14336);
#1049=PLANE('',#14337);
#1050=PLANE('',#14339);
#1051=PLANE('',#14340);
#1052=PLANE('',#14341);
#1053=PLANE('',#14342);
#1054=PLANE('',#14343);
#1055=PLANE('',#14344);
#1056=PLANE('',#14346);
#1057=PLANE('',#14347);
#1058=PLANE('',#14348);
#1059=PLANE('',#14349);
#1060=PLANE('',#14350);
#1061=PLANE('',#14351);
#1062=PLANE('',#14401);
#1063=PLANE('',#14402);
#1064=PLANE('',#14403);
#1065=PLANE('',#14404);
#1066=PLANE('',#14405);
#1067=PLANE('',#14406);
#1068=PLANE('',#14411);
#1069=PLANE('',#14416);
#1070=PLANE('',#14422);
#1071=PLANE('',#14423);
#1072=PLANE('',#14424);
#1073=PLANE('',#14425);
#1074=PLANE('',#14426);
#1075=PLANE('',#14427);
#1076=PLANE('',#14429);
#1077=PLANE('',#14430);
#1078=PLANE('',#14431);
#1079=PLANE('',#14432);
#1080=PLANE('',#14433);
#1081=PLANE('',#14434);
#1082=PLANE('',#14439);
#1083=PLANE('',#14444);
#1084=PLANE('',#14450);
#1085=PLANE('',#14451);
#1086=PLANE('',#14452);
#1087=PLANE('',#14453);
#1088=PLANE('',#14454);
#1089=PLANE('',#14455);
#1090=PLANE('',#14457);
#1091=PLANE('',#14458);
#1092=PLANE('',#14459);
#1093=PLANE('',#14460);
#1094=PLANE('',#14461);
#1095=PLANE('',#14462);
#1096=PLANE('',#14485);
#1097=PLANE('',#14486);
#1098=PLANE('',#14487);
#1099=PLANE('',#14488);
#1100=PLANE('',#14489);
#1101=PLANE('',#14490);
#1102=PLANE('',#14491);
#1103=PLANE('',#14492);
#1104=PLANE('',#14493);
#1105=PLANE('',#14494);
#1106=PLANE('',#14511);
#1107=PLANE('',#14518);
#1108=PLANE('',#14519);
#1109=PLANE('',#14536);
#1110=PLANE('',#14543);
#1111=PLANE('',#14544);
#1112=PLANE('',#14567);
#1113=PLANE('',#14568);
#1114=PLANE('',#14569);
#1115=PLANE('',#14570);
#1116=PLANE('',#14571);
#1117=PLANE('',#14572);
#1118=PLANE('',#14573);
#1119=PLANE('',#14574);
#1120=PLANE('',#14575);
#1121=PLANE('',#14576);
#1122=PLANE('',#14593);
#1123=PLANE('',#14600);
#1124=PLANE('',#14601);
#1125=PLANE('',#14618);
#1126=PLANE('',#14625);
#1127=PLANE('',#14626);
#1128=PLANE('',#14628);
#1129=PLANE('',#14629);
#1130=PLANE('',#14630);
#1131=PLANE('',#14631);
#1132=PLANE('',#14632);
#1133=PLANE('',#14633);
#1134=PLANE('',#14634);
#1135=PLANE('',#14635);
#1136=PLANE('',#14636);
#1137=PLANE('',#14637);
#1138=PLANE('',#14638);
#1139=PLANE('',#14639);
#1140=PLANE('',#14640);
#1141=PLANE('',#14641);
#1142=PLANE('',#14642);
#1143=PLANE('',#14643);
#1144=PLANE('',#14644);
#1145=PLANE('',#14645);
#1146=PLANE('',#14646);
#1147=PLANE('',#14647);
#1148=PLANE('',#14648);
#1149=PLANE('',#14649);
#1150=PLANE('',#14650);
#1151=PLANE('',#14651);
#1152=PLANE('',#14652);
#1153=PLANE('',#14653);
#1154=PLANE('',#14654);
#1155=PLANE('',#14655);
#1156=PLANE('',#14656);
#1157=PLANE('',#14657);
#1158=PLANE('',#14658);
#1159=PLANE('',#14659);
#1160=PLANE('',#14660);
#1161=PLANE('',#14661);
#1162=PLANE('',#14662);
#1163=PLANE('',#14663);
#1164=PLANE('',#14667);
#1165=PLANE('',#14668);
#1166=PLANE('',#14669);
#1167=PLANE('',#14670);
#1168=PLANE('',#14671);
#1169=PLANE('',#14672);
#1170=PLANE('',#14673);
#1171=PLANE('',#14674);
#1172=PLANE('',#14675);
#1173=PLANE('',#14676);
#1174=PLANE('',#14678);
#1175=PLANE('',#14679);
#1176=PLANE('',#14680);
#1177=PLANE('',#14682);
#1178=PLANE('',#14683);
#1179=PLANE('',#14684);
#1180=PLANE('',#14685);
#1181=PLANE('',#14686);
#1182=PLANE('',#14687);
#1183=PLANE('',#14694);
#1184=PLANE('',#14695);
#1185=PLANE('',#14696);
#1186=PLANE('',#14697);
#1187=PLANE('',#14704);
#1188=PLANE('',#14708);
#1189=PLANE('',#14713);
#1190=PLANE('',#14718);
#1191=PLANE('',#14723);
#1192=PLANE('',#14728);
#1193=PLANE('',#14738);
#1194=PLANE('',#14739);
#1195=PLANE('',#14740);
#1196=PLANE('',#14741);
#1197=PLANE('',#14742);
#1198=PLANE('',#14743);
#1199=PLANE('',#14744);
#1200=PLANE('',#14745);
#1201=PLANE('',#14746);
#1202=PLANE('',#14747);
#1203=PLANE('',#14748);
#1204=PLANE('',#14749);
#1205=PLANE('',#14750);
#1206=PLANE('',#14751);
#1207=PLANE('',#14753);
#1208=PLANE('',#14761);
#1209=PLANE('',#14769);
#1210=PLANE('',#14770);
#1211=PLANE('',#14771);
#1212=PLANE('',#14772);
#1213=PLANE('',#14773);
#1214=PLANE('',#14774);
#1215=PLANE('',#14775);
#1216=PLANE('',#14776);
#1217=PLANE('',#14777);
#1218=PLANE('',#14793);
#1219=PLANE('',#14796);
#1220=PLANE('',#14808);
#1221=PLANE('',#14817);
#1222=PLANE('',#14848);
#1223=PLANE('',#14853);
#1224=PLANE('',#14858);
#1225=PLANE('',#14864);
#1226=PLANE('',#14869);
#1227=PLANE('',#14878);
#1228=PLANE('',#14882);
#1229=PLANE('',#14883);
#1230=PLANE('',#14885);
#1231=PLANE('',#14890);
#1232=PLANE('',#14893);
#1233=PLANE('',#14898);
#1234=PLANE('',#14907);
#1235=PLANE('',#14908);
#1236=PLANE('',#14909);
#1237=PLANE('',#14910);
#1238=PLANE('',#14911);
#1239=PLANE('',#14912);
#1240=PLANE('',#14913);
#1241=PLANE('',#14914);
#1242=PLANE('',#14915);
#1243=PLANE('',#14917);
#1244=PLANE('',#14925);
#1245=PLANE('',#14956);
#1246=PLANE('',#14957);
#1247=PLANE('',#14958);
#1248=PLANE('',#14959);
#1249=PLANE('',#14960);
#1250=PLANE('',#14961);
#1251=PLANE('',#14966);
#1252=PLANE('',#14970);
#1253=PLANE('',#14974);
#1254=PLANE('',#14978);
#1255=PLANE('',#14979);
#1256=PLANE('',#14980);
#1257=PLANE('',#14981);
#1258=PLANE('',#14982);
#1259=PLANE('',#14983);
#1260=PLANE('',#14984);
#1261=PLANE('',#14985);
#1262=PLANE('',#14986);
#1263=PLANE('',#14987);
#1264=PLANE('',#14988);
#1265=PLANE('',#14989);
#1266=PLANE('',#14990);
#1267=PLANE('',#14991);
#1268=PLANE('',#14992);
#1269=PLANE('',#14993);
#1270=PLANE('',#14994);
#1271=PLANE('',#14995);
#1272=PLANE('',#14996);
#1273=PLANE('',#14997);
#1274=PLANE('',#14998);
#1275=PLANE('',#14999);
#1276=PLANE('',#15000);
#1277=PLANE('',#15001);
#1278=PLANE('',#15002);
#1279=PLANE('',#15003);
#1280=PLANE('',#15004);
#1281=PLANE('',#15005);
#1282=PLANE('',#15006);
#1283=PLANE('',#15007);
#1284=PLANE('',#15008);
#1285=PLANE('',#15009);
#1286=PLANE('',#15010);
#1287=PLANE('',#15011);
#1288=PLANE('',#15012);
#1289=PLANE('',#15013);
#1290=PLANE('',#15014);
#1291=PLANE('',#15015);
#1292=PLANE('',#15016);
#1293=PLANE('',#15017);
#1294=PLANE('',#15018);
#1295=PLANE('',#15019);
#1296=PLANE('',#15020);
#1297=PLANE('',#15021);
#1298=PLANE('',#15022);
#1299=PLANE('',#15023);
#1300=PLANE('',#15024);
#1301=PLANE('',#15025);
#1302=PLANE('',#15026);
#1303=PLANE('',#15027);
#1304=PLANE('',#15028);
#1305=PLANE('',#15029);
#1306=PLANE('',#15030);
#1307=PLANE('',#15031);
#1308=PLANE('',#15032);
#1309=PLANE('',#15033);
#1310=PLANE('',#15034);
#1311=PLANE('',#15035);
#1312=PLANE('',#15036);
#1313=PLANE('',#15037);
#1314=PLANE('',#15038);
#1315=PLANE('',#15039);
#1316=PLANE('',#15040);
#1317=PLANE('',#15041);
#1318=PLANE('',#15042);
#1319=PLANE('',#15043);
#1320=PLANE('',#15044);
#1321=PLANE('',#15045);
#1322=PLANE('',#15046);
#1323=PLANE('',#15047);
#1324=PLANE('',#15048);
#1325=PLANE('',#15049);
#1326=PLANE('',#15050);
#1327=PLANE('',#15051);
#1328=PLANE('',#15052);
#1329=PLANE('',#15053);
#1330=PLANE('',#15054);
#1331=PLANE('',#15055);
#1332=PLANE('',#15056);
#1333=PLANE('',#15057);
#1334=PLANE('',#15058);
#1335=PLANE('',#15059);
#1336=PLANE('',#15060);
#1337=PLANE('',#15061);
#1338=PLANE('',#15062);
#1339=PLANE('',#15063);
#1340=PLANE('',#15064);
#1341=PLANE('',#15065);
#1342=PLANE('',#15066);
#1343=PLANE('',#15067);
#1344=PLANE('',#15068);
#1345=PLANE('',#15069);
#1346=PLANE('',#15070);
#1347=PLANE('',#15071);
#1348=PLANE('',#15072);
#1349=PLANE('',#15073);
#1350=PLANE('',#15074);
#1351=PLANE('',#15075);
#1352=PLANE('',#15076);
#1353=PLANE('',#15077);
#1354=PLANE('',#15078);
#1355=PLANE('',#15079);
#1356=PLANE('',#15080);
#1357=PLANE('',#15081);
#1358=PLANE('',#15082);
#1359=PLANE('',#15083);
#1360=PLANE('',#15084);
#1361=PLANE('',#15085);
#1362=PLANE('',#15086);
#1363=PLANE('',#15087);
#1364=PLANE('',#15088);
#1365=PLANE('',#15089);
#1366=PLANE('',#15090);
#1367=PLANE('',#15091);
#1368=PLANE('',#15092);
#1369=PLANE('',#15093);
#1370=PLANE('',#15094);
#1371=PLANE('',#15095);
#1372=PLANE('',#15096);
#1373=PLANE('',#15097);
#1374=PLANE('',#15098);
#1375=PLANE('',#15099);
#1376=PLANE('',#15100);
#1377=PLANE('',#15101);
#1378=PLANE('',#15102);
#1379=PLANE('',#15103);
#1380=PLANE('',#15104);
#1381=PLANE('',#15105);
#1382=PLANE('',#15106);
#1383=PLANE('',#15107);
#1384=PLANE('',#15108);
#1385=PLANE('',#15111);
#1386=PLANE('',#15117);
#1387=PLANE('',#15123);
#1388=PLANE('',#15129);
#1389=PLANE('',#15135);
#1390=PLANE('',#15136);
#1391=PLANE('',#15137);
#1392=PLANE('',#15138);
#1393=PLANE('',#15139);
#1394=PLANE('',#15140);
#1395=PLANE('',#15141);
#1396=PLANE('',#15142);
#1397=PLANE('',#15143);
#1398=PLANE('',#15144);
#1399=PLANE('',#15145);
#1400=PLANE('',#15146);
#1401=PLANE('',#15147);
#1402=PLANE('',#15148);
#1403=PLANE('',#15150);
#1404=PLANE('',#15151);
#1405=PLANE('',#15152);
#1406=PLANE('',#15153);
#1407=PLANE('',#15154);
#1408=PLANE('',#15155);
#1409=PLANE('',#15156);
#1410=PLANE('',#15157);
#1411=PLANE('',#15158);
#1412=PLANE('',#15159);
#1413=PLANE('',#15161);
#1414=PLANE('',#15162);
#1415=PLANE('',#15163);
#1416=PLANE('',#15164);
#1417=PLANE('',#15165);
#1418=PLANE('',#15166);
#1419=PLANE('',#15167);
#1420=PLANE('',#15168);
#1421=PLANE('',#15169);
#1422=PLANE('',#15170);
#1423=PLANE('',#15175);
#1424=PLANE('',#15176);
#1425=PLANE('',#15177);
#1426=PLANE('',#15178);
#1427=PLANE('',#15179);
#1428=PLANE('',#15180);
#1429=PLANE('',#15181);
#1430=PLANE('',#15182);
#1431=PLANE('',#15183);
#1432=PLANE('',#15185);
#1433=PLANE('',#15193);
#1434=PLANE('',#15200);
#1435=PLANE('',#15201);
#1436=PLANE('',#15203);
#1437=PLANE('',#15204);
#1438=PLANE('',#15205);
#1439=PLANE('',#15210);
#1440=PLANE('',#15214);
#1441=PLANE('',#15215);
#1442=PLANE('',#15216);
#1443=PLANE('',#15218);
#1444=PLANE('',#15219);
#1445=PLANE('',#15220);
#1446=PLANE('',#15222);
#1447=PLANE('',#15225);
#1448=PLANE('',#15233);
#1449=PLANE('',#15234);
#1450=PLANE('',#15242);
#1451=PLANE('',#15243);
#1452=PLANE('',#15251);
#1453=PLANE('',#15252);
#1454=PLANE('',#15260);
#1455=PLANE('',#15261);
#1456=PLANE('',#15269);
#1457=PLANE('',#15270);
#1458=PLANE('',#15278);
#1459=PLANE('',#15279);
#1460=PLANE('',#15287);
#1461=PLANE('',#15288);
#1462=PLANE('',#15293);
#1463=PLANE('',#15294);
#1464=PLANE('',#15295);
#1465=PLANE('',#15296);
#1466=PLANE('',#15304);
#1467=PLANE('',#15305);
#1468=PLANE('',#15307);
#1469=PLANE('',#15308);
#1470=PLANE('',#15312);
#1471=PLANE('',#15320);
#1472=PLANE('',#15321);
#1473=PLANE('',#15323);
#1474=PLANE('',#15324);
#1475=PLANE('',#15325);
#1476=PLANE('',#15326);
#1477=PLANE('',#15353);
#1478=PLANE('',#15354);
#1479=PLANE('',#15357);
#1480=PLANE('',#15360);
#1481=PLANE('',#15363);
#1482=PLANE('',#15366);
#1483=PLANE('',#15369);
#1484=PLANE('',#15372);
#1485=PLANE('',#15375);
#1486=PLANE('',#15378);
#1487=PLANE('',#15381);
#1488=PLANE('',#15384);
#1489=PLANE('',#15387);
#1490=PLANE('',#15390);
#1491=PLANE('',#15393);
#1492=PLANE('',#15396);
#1493=PLANE('',#15399);
#1494=PLANE('',#15402);
#1495=PLANE('',#15405);
#1496=PLANE('',#15408);
#1497=PLANE('',#15411);
#1498=PLANE('',#15412);
#1499=PLANE('',#15416);
#1500=PLANE('',#15424);
#1501=PLANE('',#15432);
#1502=PLANE('',#15433);
#1503=PLANE('',#15434);
#1504=PLANE('',#15435);
#1505=PLANE('',#15436);
#1506=PLANE('',#15437);
#1507=PLANE('',#15438);
#1508=PLANE('',#15439);
#1509=PLANE('',#15440);
#1510=PLANE('',#15524);
#1511=PLANE('',#15525);
#1512=PLANE('',#15526);
#1513=PLANE('',#15527);
#1514=PLANE('',#15528);
#1515=PLANE('',#15529);
#1516=PLANE('',#15530);
#1517=PLANE('',#15531);
#1518=PLANE('',#15532);
#1519=PLANE('',#15533);
#1520=PLANE('',#15541);
#1521=PLANE('',#15542);
#1522=PLANE('',#15544);
#1523=PLANE('',#15552);
#1524=PLANE('',#15560);
#1525=PLANE('',#15561);
#1526=PLANE('',#15562);
#1527=PLANE('',#15563);
#1528=PLANE('',#15564);
#1529=PLANE('',#15565);
#1530=PLANE('',#15566);
#1531=PLANE('',#15567);
#1532=PLANE('',#15568);
#1533=PLANE('',#15593);
#1534=PLANE('',#15594);
#1535=FACE_OUTER_BOUND('',#2274,.T.);
#1536=FACE_OUTER_BOUND('',#2275,.T.);
#1537=FACE_OUTER_BOUND('',#2276,.T.);
#1538=FACE_OUTER_BOUND('',#2277,.T.);
#1539=FACE_OUTER_BOUND('',#2278,.T.);
#1540=FACE_OUTER_BOUND('',#2279,.T.);
#1541=FACE_OUTER_BOUND('',#2280,.T.);
#1542=FACE_OUTER_BOUND('',#2281,.T.);
#1543=FACE_OUTER_BOUND('',#2282,.T.);
#1544=FACE_OUTER_BOUND('',#2287,.T.);
#1545=FACE_OUTER_BOUND('',#2292,.T.);
#1546=FACE_OUTER_BOUND('',#2293,.T.);
#1547=FACE_OUTER_BOUND('',#2294,.T.);
#1548=FACE_OUTER_BOUND('',#2295,.T.);
#1549=FACE_OUTER_BOUND('',#2296,.T.);
#1550=FACE_OUTER_BOUND('',#2297,.T.);
#1551=FACE_OUTER_BOUND('',#2298,.T.);
#1552=FACE_OUTER_BOUND('',#2299,.T.);
#1553=FACE_OUTER_BOUND('',#2300,.T.);
#1554=FACE_OUTER_BOUND('',#2301,.T.);
#1555=FACE_OUTER_BOUND('',#2302,.T.);
#1556=FACE_OUTER_BOUND('',#2303,.T.);
#1557=FACE_OUTER_BOUND('',#2304,.T.);
#1558=FACE_OUTER_BOUND('',#2305,.T.);
#1559=FACE_OUTER_BOUND('',#2306,.T.);
#1560=FACE_OUTER_BOUND('',#2307,.T.);
#1561=FACE_OUTER_BOUND('',#2308,.T.);
#1562=FACE_OUTER_BOUND('',#2309,.T.);
#1563=FACE_OUTER_BOUND('',#2310,.T.);
#1564=FACE_OUTER_BOUND('',#2311,.T.);
#1565=FACE_OUTER_BOUND('',#2312,.T.);
#1566=FACE_OUTER_BOUND('',#2313,.T.);
#1567=FACE_OUTER_BOUND('',#2314,.T.);
#1568=FACE_OUTER_BOUND('',#2315,.T.);
#1569=FACE_OUTER_BOUND('',#2316,.T.);
#1570=FACE_OUTER_BOUND('',#2317,.T.);
#1571=FACE_OUTER_BOUND('',#2318,.T.);
#1572=FACE_OUTER_BOUND('',#2319,.T.);
#1573=FACE_OUTER_BOUND('',#2320,.T.);
#1574=FACE_OUTER_BOUND('',#2321,.T.);
#1575=FACE_OUTER_BOUND('',#2322,.T.);
#1576=FACE_OUTER_BOUND('',#2323,.T.);
#1577=FACE_OUTER_BOUND('',#2324,.T.);
#1578=FACE_OUTER_BOUND('',#2341,.T.);
#1579=FACE_OUTER_BOUND('',#2358,.T.);
#1580=FACE_OUTER_BOUND('',#2359,.T.);
#1581=FACE_OUTER_BOUND('',#2361,.T.);
#1582=FACE_OUTER_BOUND('',#2362,.T.);
#1583=FACE_OUTER_BOUND('',#2364,.T.);
#1584=FACE_OUTER_BOUND('',#2365,.T.);
#1585=FACE_OUTER_BOUND('',#2366,.T.);
#1586=FACE_OUTER_BOUND('',#2367,.T.);
#1587=FACE_OUTER_BOUND('',#2368,.T.);
#1588=FACE_OUTER_BOUND('',#2369,.T.);
#1589=FACE_OUTER_BOUND('',#2370,.T.);
#1590=FACE_OUTER_BOUND('',#2373,.T.);
#1591=FACE_OUTER_BOUND('',#2376,.T.);
#1592=FACE_OUTER_BOUND('',#2377,.T.);
#1593=FACE_OUTER_BOUND('',#2378,.T.);
#1594=FACE_OUTER_BOUND('',#2379,.T.);
#1595=FACE_OUTER_BOUND('',#2380,.T.);
#1596=FACE_OUTER_BOUND('',#2381,.T.);
#1597=FACE_OUTER_BOUND('',#2382,.T.);
#1598=FACE_OUTER_BOUND('',#2383,.T.);
#1599=FACE_OUTER_BOUND('',#2385,.T.);
#1600=FACE_OUTER_BOUND('',#2386,.T.);
#1601=FACE_OUTER_BOUND('',#2388,.T.);
#1602=FACE_OUTER_BOUND('',#2389,.T.);
#1603=FACE_OUTER_BOUND('',#2390,.T.);
#1604=FACE_OUTER_BOUND('',#2391,.T.);
#1605=FACE_OUTER_BOUND('',#2392,.T.);
#1606=FACE_OUTER_BOUND('',#2393,.T.);
#1607=FACE_OUTER_BOUND('',#2394,.T.);
#1608=FACE_OUTER_BOUND('',#2397,.T.);
#1609=FACE_OUTER_BOUND('',#2400,.T.);
#1610=FACE_OUTER_BOUND('',#2401,.T.);
#1611=FACE_OUTER_BOUND('',#2402,.T.);
#1612=FACE_OUTER_BOUND('',#2403,.T.);
#1613=FACE_OUTER_BOUND('',#2404,.T.);
#1614=FACE_OUTER_BOUND('',#2405,.T.);
#1615=FACE_OUTER_BOUND('',#2406,.T.);
#1616=FACE_OUTER_BOUND('',#2407,.T.);
#1617=FACE_OUTER_BOUND('',#2408,.T.);
#1618=FACE_OUTER_BOUND('',#2409,.T.);
#1619=FACE_OUTER_BOUND('',#2410,.T.);
#1620=FACE_OUTER_BOUND('',#2411,.T.);
#1621=FACE_OUTER_BOUND('',#2412,.T.);
#1622=FACE_OUTER_BOUND('',#2413,.T.);
#1623=FACE_OUTER_BOUND('',#2415,.T.);
#1624=FACE_OUTER_BOUND('',#2417,.T.);
#1625=FACE_OUTER_BOUND('',#2418,.T.);
#1626=FACE_OUTER_BOUND('',#2419,.T.);
#1627=FACE_OUTER_BOUND('',#2425,.T.);
#1628=FACE_OUTER_BOUND('',#2426,.T.);
#1629=FACE_OUTER_BOUND('',#2432,.T.);
#1630=FACE_OUTER_BOUND('',#2433,.T.);
#1631=FACE_OUTER_BOUND('',#2434,.T.);
#1632=FACE_OUTER_BOUND('',#2437,.T.);
#1633=FACE_OUTER_BOUND('',#2438,.T.);
#1634=FACE_OUTER_BOUND('',#2439,.T.);
#1635=FACE_OUTER_BOUND('',#2440,.T.);
#1636=FACE_OUTER_BOUND('',#2441,.T.);
#1637=FACE_OUTER_BOUND('',#2442,.T.);
#1638=FACE_OUTER_BOUND('',#2444,.T.);
#1639=FACE_OUTER_BOUND('',#2445,.T.);
#1640=FACE_OUTER_BOUND('',#2446,.T.);
#1641=FACE_OUTER_BOUND('',#2452,.T.);
#1642=FACE_OUTER_BOUND('',#2458,.T.);
#1643=FACE_OUTER_BOUND('',#2459,.T.);
#1644=FACE_OUTER_BOUND('',#2460,.T.);
#1645=FACE_OUTER_BOUND('',#2461,.T.);
#1646=FACE_OUTER_BOUND('',#2462,.T.);
#1647=FACE_OUTER_BOUND('',#2463,.T.);
#1648=FACE_OUTER_BOUND('',#2465,.T.);
#1649=FACE_OUTER_BOUND('',#2466,.T.);
#1650=FACE_OUTER_BOUND('',#2467,.T.);
#1651=FACE_OUTER_BOUND('',#2473,.T.);
#1652=FACE_OUTER_BOUND('',#2479,.T.);
#1653=FACE_OUTER_BOUND('',#2480,.T.);
#1654=FACE_OUTER_BOUND('',#2481,.T.);
#1655=FACE_OUTER_BOUND('',#2482,.T.);
#1656=FACE_OUTER_BOUND('',#2483,.T.);
#1657=FACE_OUTER_BOUND('',#2484,.T.);
#1658=FACE_OUTER_BOUND('',#2485,.T.);
#1659=FACE_OUTER_BOUND('',#2486,.T.);
#1660=FACE_OUTER_BOUND('',#2488,.T.);
#1661=FACE_OUTER_BOUND('',#2490,.T.);
#1662=FACE_OUTER_BOUND('',#2491,.T.);
#1663=FACE_OUTER_BOUND('',#2492,.T.);
#1664=FACE_OUTER_BOUND('',#2498,.T.);
#1665=FACE_OUTER_BOUND('',#2499,.T.);
#1666=FACE_OUTER_BOUND('',#2505,.T.);
#1667=FACE_OUTER_BOUND('',#2506,.T.);
#1668=FACE_OUTER_BOUND('',#2507,.T.);
#1669=FACE_OUTER_BOUND('',#2510,.T.);
#1670=FACE_OUTER_BOUND('',#2511,.T.);
#1671=FACE_OUTER_BOUND('',#2512,.T.);
#1672=FACE_OUTER_BOUND('',#2513,.T.);
#1673=FACE_OUTER_BOUND('',#2514,.T.);
#1674=FACE_OUTER_BOUND('',#2515,.T.);
#1675=FACE_OUTER_BOUND('',#2517,.T.);
#1676=FACE_OUTER_BOUND('',#2518,.T.);
#1677=FACE_OUTER_BOUND('',#2519,.T.);
#1678=FACE_OUTER_BOUND('',#2525,.T.);
#1679=FACE_OUTER_BOUND('',#2531,.T.);
#1680=FACE_OUTER_BOUND('',#2532,.T.);
#1681=FACE_OUTER_BOUND('',#2533,.T.);
#1682=FACE_OUTER_BOUND('',#2534,.T.);
#1683=FACE_OUTER_BOUND('',#2535,.T.);
#1684=FACE_OUTER_BOUND('',#2536,.T.);
#1685=FACE_OUTER_BOUND('',#2538,.T.);
#1686=FACE_OUTER_BOUND('',#2539,.T.);
#1687=FACE_OUTER_BOUND('',#2540,.T.);
#1688=FACE_OUTER_BOUND('',#2546,.T.);
#1689=FACE_OUTER_BOUND('',#2552,.T.);
#1690=FACE_OUTER_BOUND('',#2553,.T.);
#1691=FACE_OUTER_BOUND('',#2554,.T.);
#1692=FACE_OUTER_BOUND('',#2555,.T.);
#1693=FACE_OUTER_BOUND('',#2556,.T.);
#1694=FACE_OUTER_BOUND('',#2557,.T.);
#1695=FACE_OUTER_BOUND('',#2558,.T.);
#1696=FACE_OUTER_BOUND('',#2559,.T.);
#1697=FACE_OUTER_BOUND('',#2560,.T.);
#1698=FACE_OUTER_BOUND('',#2561,.T.);
#1699=FACE_OUTER_BOUND('',#2562,.T.);
#1700=FACE_OUTER_BOUND('',#2563,.T.);
#1701=FACE_OUTER_BOUND('',#2564,.T.);
#1702=FACE_OUTER_BOUND('',#2565,.T.);
#1703=FACE_OUTER_BOUND('',#2566,.T.);
#1704=FACE_OUTER_BOUND('',#2567,.T.);
#1705=FACE_OUTER_BOUND('',#2568,.T.);
#1706=FACE_OUTER_BOUND('',#2569,.T.);
#1707=FACE_OUTER_BOUND('',#2570,.T.);
#1708=FACE_OUTER_BOUND('',#2571,.T.);
#1709=FACE_OUTER_BOUND('',#2572,.T.);
#1710=FACE_OUTER_BOUND('',#2573,.T.);
#1711=FACE_OUTER_BOUND('',#2574,.T.);
#1712=FACE_OUTER_BOUND('',#2575,.T.);
#1713=FACE_OUTER_BOUND('',#2576,.T.);
#1714=FACE_OUTER_BOUND('',#2577,.T.);
#1715=FACE_OUTER_BOUND('',#2578,.T.);
#1716=FACE_OUTER_BOUND('',#2579,.T.);
#1717=FACE_OUTER_BOUND('',#2580,.T.);
#1718=FACE_OUTER_BOUND('',#2581,.T.);
#1719=FACE_OUTER_BOUND('',#2582,.T.);
#1720=FACE_OUTER_BOUND('',#2583,.T.);
#1721=FACE_OUTER_BOUND('',#2584,.T.);
#1722=FACE_OUTER_BOUND('',#2585,.T.);
#1723=FACE_OUTER_BOUND('',#2586,.T.);
#1724=FACE_OUTER_BOUND('',#2587,.T.);
#1725=FACE_OUTER_BOUND('',#2588,.T.);
#1726=FACE_OUTER_BOUND('',#2589,.T.);
#1727=FACE_OUTER_BOUND('',#2590,.T.);
#1728=FACE_OUTER_BOUND('',#2591,.T.);
#1729=FACE_OUTER_BOUND('',#2592,.T.);
#1730=FACE_OUTER_BOUND('',#2593,.T.);
#1731=FACE_OUTER_BOUND('',#2594,.T.);
#1732=FACE_OUTER_BOUND('',#2595,.T.);
#1733=FACE_OUTER_BOUND('',#2596,.T.);
#1734=FACE_OUTER_BOUND('',#2597,.T.);
#1735=FACE_OUTER_BOUND('',#2599,.T.);
#1736=FACE_OUTER_BOUND('',#2601,.T.);
#1737=FACE_OUTER_BOUND('',#2602,.T.);
#1738=FACE_OUTER_BOUND('',#2603,.T.);
#1739=FACE_OUTER_BOUND('',#2605,.T.);
#1740=FACE_OUTER_BOUND('',#2606,.T.);
#1741=FACE_OUTER_BOUND('',#2607,.T.);
#1742=FACE_OUTER_BOUND('',#2608,.T.);
#1743=FACE_OUTER_BOUND('',#2609,.T.);
#1744=FACE_OUTER_BOUND('',#2610,.T.);
#1745=FACE_OUTER_BOUND('',#2611,.T.);
#1746=FACE_OUTER_BOUND('',#2612,.T.);
#1747=FACE_OUTER_BOUND('',#2613,.T.);
#1748=FACE_OUTER_BOUND('',#2614,.T.);
#1749=FACE_OUTER_BOUND('',#2615,.T.);
#1750=FACE_OUTER_BOUND('',#2616,.T.);
#1751=FACE_OUTER_BOUND('',#2617,.T.);
#1752=FACE_OUTER_BOUND('',#2618,.T.);
#1753=FACE_OUTER_BOUND('',#2620,.T.);
#1754=FACE_OUTER_BOUND('',#2621,.T.);
#1755=FACE_OUTER_BOUND('',#2623,.T.);
#1756=FACE_OUTER_BOUND('',#2624,.T.);
#1757=FACE_OUTER_BOUND('',#2626,.T.);
#1758=FACE_OUTER_BOUND('',#2627,.T.);
#1759=FACE_OUTER_BOUND('',#2629,.T.);
#1760=FACE_OUTER_BOUND('',#2630,.T.);
#1761=FACE_OUTER_BOUND('',#2632,.T.);
#1762=FACE_OUTER_BOUND('',#2633,.T.);
#1763=FACE_OUTER_BOUND('',#2635,.T.);
#1764=FACE_OUTER_BOUND('',#2636,.T.);
#1765=FACE_OUTER_BOUND('',#2637,.T.);
#1766=FACE_OUTER_BOUND('',#2638,.T.);
#1767=FACE_OUTER_BOUND('',#2639,.T.);
#1768=FACE_OUTER_BOUND('',#2640,.T.);
#1769=FACE_OUTER_BOUND('',#2641,.T.);
#1770=FACE_OUTER_BOUND('',#2642,.T.);
#1771=FACE_OUTER_BOUND('',#2643,.T.);
#1772=FACE_OUTER_BOUND('',#2648,.T.);
#1773=FACE_OUTER_BOUND('',#2649,.T.);
#1774=FACE_OUTER_BOUND('',#2650,.T.);
#1775=FACE_OUTER_BOUND('',#2651,.T.);
#1776=FACE_OUTER_BOUND('',#2652,.T.);
#1777=FACE_OUTER_BOUND('',#2653,.T.);
#1778=FACE_OUTER_BOUND('',#2658,.T.);
#1779=FACE_OUTER_BOUND('',#2659,.T.);
#1780=FACE_OUTER_BOUND('',#2660,.T.);
#1781=FACE_OUTER_BOUND('',#2661,.T.);
#1782=FACE_OUTER_BOUND('',#2662,.T.);
#1783=FACE_OUTER_BOUND('',#2663,.T.);
#1784=FACE_OUTER_BOUND('',#2664,.T.);
#1785=FACE_OUTER_BOUND('',#2665,.T.);
#1786=FACE_OUTER_BOUND('',#2667,.T.);
#1787=FACE_OUTER_BOUND('',#2668,.T.);
#1788=FACE_OUTER_BOUND('',#2669,.T.);
#1789=FACE_OUTER_BOUND('',#2670,.T.);
#1790=FACE_OUTER_BOUND('',#2671,.T.);
#1791=FACE_OUTER_BOUND('',#2672,.T.);
#1792=FACE_OUTER_BOUND('',#2673,.T.);
#1793=FACE_OUTER_BOUND('',#2674,.T.);
#1794=FACE_OUTER_BOUND('',#2675,.T.);
#1795=FACE_OUTER_BOUND('',#2676,.T.);
#1796=FACE_OUTER_BOUND('',#2677,.T.);
#1797=FACE_OUTER_BOUND('',#2678,.T.);
#1798=FACE_OUTER_BOUND('',#2679,.T.);
#1799=FACE_OUTER_BOUND('',#2680,.T.);
#1800=FACE_OUTER_BOUND('',#2681,.T.);
#1801=FACE_OUTER_BOUND('',#2682,.T.);
#1802=FACE_OUTER_BOUND('',#2683,.T.);
#1803=FACE_OUTER_BOUND('',#2685,.T.);
#1804=FACE_OUTER_BOUND('',#2686,.T.);
#1805=FACE_OUTER_BOUND('',#2688,.T.);
#1806=FACE_OUTER_BOUND('',#2689,.T.);
#1807=FACE_OUTER_BOUND('',#2690,.T.);
#1808=FACE_OUTER_BOUND('',#2691,.T.);
#1809=FACE_OUTER_BOUND('',#2693,.T.);
#1810=FACE_OUTER_BOUND('',#2694,.T.);
#1811=FACE_OUTER_BOUND('',#2695,.T.);
#1812=FACE_OUTER_BOUND('',#2696,.T.);
#1813=FACE_OUTER_BOUND('',#2698,.T.);
#1814=FACE_OUTER_BOUND('',#2699,.T.);
#1815=FACE_OUTER_BOUND('',#2700,.T.);
#1816=FACE_OUTER_BOUND('',#2701,.T.);
#1817=FACE_OUTER_BOUND('',#2702,.T.);
#1818=FACE_OUTER_BOUND('',#2703,.T.);
#1819=FACE_OUTER_BOUND('',#2704,.T.);
#1820=FACE_OUTER_BOUND('',#2705,.T.);
#1821=FACE_OUTER_BOUND('',#2706,.T.);
#1822=FACE_OUTER_BOUND('',#2707,.T.);
#1823=FACE_OUTER_BOUND('',#2708,.T.);
#1824=FACE_OUTER_BOUND('',#2709,.T.);
#1825=FACE_OUTER_BOUND('',#2710,.T.);
#1826=FACE_OUTER_BOUND('',#2711,.T.);
#1827=FACE_OUTER_BOUND('',#2712,.T.);
#1828=FACE_OUTER_BOUND('',#2713,.T.);
#1829=FACE_OUTER_BOUND('',#2714,.T.);
#1830=FACE_OUTER_BOUND('',#2715,.T.);
#1831=FACE_OUTER_BOUND('',#2716,.T.);
#1832=FACE_OUTER_BOUND('',#2717,.T.);
#1833=FACE_OUTER_BOUND('',#2718,.T.);
#1834=FACE_OUTER_BOUND('',#2719,.T.);
#1835=FACE_OUTER_BOUND('',#2720,.T.);
#1836=FACE_OUTER_BOUND('',#2721,.T.);
#1837=FACE_OUTER_BOUND('',#2723,.T.);
#1838=FACE_OUTER_BOUND('',#2724,.T.);
#1839=FACE_OUTER_BOUND('',#2726,.T.);
#1840=FACE_OUTER_BOUND('',#2727,.T.);
#1841=FACE_OUTER_BOUND('',#2729,.T.);
#1842=FACE_OUTER_BOUND('',#2730,.T.);
#1843=FACE_OUTER_BOUND('',#2732,.T.);
#1844=FACE_OUTER_BOUND('',#2733,.T.);
#1845=FACE_OUTER_BOUND('',#2735,.T.);
#1846=FACE_OUTER_BOUND('',#2736,.T.);
#1847=FACE_OUTER_BOUND('',#2737,.T.);
#1848=FACE_OUTER_BOUND('',#2738,.T.);
#1849=FACE_OUTER_BOUND('',#2739,.T.);
#1850=FACE_OUTER_BOUND('',#2740,.T.);
#1851=FACE_OUTER_BOUND('',#2741,.T.);
#1852=FACE_OUTER_BOUND('',#2742,.T.);
#1853=FACE_OUTER_BOUND('',#2743,.T.);
#1854=FACE_OUTER_BOUND('',#2744,.T.);
#1855=FACE_OUTER_BOUND('',#2745,.T.);
#1856=FACE_OUTER_BOUND('',#2746,.T.);
#1857=FACE_OUTER_BOUND('',#2747,.T.);
#1858=FACE_OUTER_BOUND('',#2748,.T.);
#1859=FACE_OUTER_BOUND('',#2749,.T.);
#1860=FACE_OUTER_BOUND('',#2751,.T.);
#1861=FACE_OUTER_BOUND('',#2752,.T.);
#1862=FACE_OUTER_BOUND('',#2753,.T.);
#1863=FACE_OUTER_BOUND('',#2754,.T.);
#1864=FACE_OUTER_BOUND('',#2755,.T.);
#1865=FACE_OUTER_BOUND('',#2756,.T.);
#1866=FACE_OUTER_BOUND('',#2757,.T.);
#1867=FACE_OUTER_BOUND('',#2758,.T.);
#1868=FACE_OUTER_BOUND('',#2759,.T.);
#1869=FACE_OUTER_BOUND('',#2760,.T.);
#1870=FACE_OUTER_BOUND('',#2761,.T.);
#1871=FACE_OUTER_BOUND('',#2762,.T.);
#1872=FACE_OUTER_BOUND('',#2763,.T.);
#1873=FACE_OUTER_BOUND('',#2764,.T.);
#1874=FACE_OUTER_BOUND('',#2765,.T.);
#1875=FACE_OUTER_BOUND('',#2774,.T.);
#1876=FACE_OUTER_BOUND('',#2783,.T.);
#1877=FACE_OUTER_BOUND('',#2784,.T.);
#1878=FACE_OUTER_BOUND('',#2785,.T.);
#1879=FACE_OUTER_BOUND('',#2786,.T.);
#1880=FACE_OUTER_BOUND('',#2787,.T.);
#1881=FACE_OUTER_BOUND('',#2788,.T.);
#1882=FACE_OUTER_BOUND('',#2789,.T.);
#1883=FACE_OUTER_BOUND('',#2790,.T.);
#1884=FACE_OUTER_BOUND('',#2791,.T.);
#1885=FACE_OUTER_BOUND('',#2792,.T.);
#1886=FACE_OUTER_BOUND('',#2797,.T.);
#1887=FACE_OUTER_BOUND('',#2798,.T.);
#1888=FACE_OUTER_BOUND('',#2799,.T.);
#1889=FACE_OUTER_BOUND('',#2800,.T.);
#1890=FACE_OUTER_BOUND('',#2801,.T.);
#1891=FACE_OUTER_BOUND('',#2802,.T.);
#1892=FACE_OUTER_BOUND('',#2803,.T.);
#1893=FACE_OUTER_BOUND('',#2804,.T.);
#1894=FACE_OUTER_BOUND('',#2805,.T.);
#1895=FACE_OUTER_BOUND('',#2806,.T.);
#1896=FACE_OUTER_BOUND('',#2807,.T.);
#1897=FACE_OUTER_BOUND('',#2808,.T.);
#1898=FACE_OUTER_BOUND('',#2809,.T.);
#1899=FACE_OUTER_BOUND('',#2810,.T.);
#1900=FACE_OUTER_BOUND('',#2811,.T.);
#1901=FACE_OUTER_BOUND('',#2812,.T.);
#1902=FACE_OUTER_BOUND('',#2813,.T.);
#1903=FACE_OUTER_BOUND('',#2814,.T.);
#1904=FACE_OUTER_BOUND('',#2815,.T.);
#1905=FACE_OUTER_BOUND('',#2816,.T.);
#1906=FACE_OUTER_BOUND('',#2817,.T.);
#1907=FACE_OUTER_BOUND('',#2818,.T.);
#1908=FACE_OUTER_BOUND('',#2819,.T.);
#1909=FACE_OUTER_BOUND('',#2820,.T.);
#1910=FACE_OUTER_BOUND('',#2821,.T.);
#1911=FACE_OUTER_BOUND('',#2822,.T.);
#1912=FACE_OUTER_BOUND('',#2823,.T.);
#1913=FACE_OUTER_BOUND('',#2824,.T.);
#1914=FACE_OUTER_BOUND('',#2825,.T.);
#1915=FACE_OUTER_BOUND('',#2826,.T.);
#1916=FACE_OUTER_BOUND('',#2827,.T.);
#1917=FACE_OUTER_BOUND('',#2828,.T.);
#1918=FACE_OUTER_BOUND('',#2829,.T.);
#1919=FACE_OUTER_BOUND('',#2830,.T.);
#1920=FACE_OUTER_BOUND('',#2831,.T.);
#1921=FACE_OUTER_BOUND('',#2832,.T.);
#1922=FACE_OUTER_BOUND('',#2833,.T.);
#1923=FACE_OUTER_BOUND('',#2834,.T.);
#1924=FACE_OUTER_BOUND('',#2835,.T.);
#1925=FACE_OUTER_BOUND('',#2836,.T.);
#1926=FACE_OUTER_BOUND('',#2837,.T.);
#1927=FACE_OUTER_BOUND('',#2838,.T.);
#1928=FACE_OUTER_BOUND('',#2839,.T.);
#1929=FACE_OUTER_BOUND('',#2840,.T.);
#1930=FACE_OUTER_BOUND('',#2841,.T.);
#1931=FACE_OUTER_BOUND('',#2842,.T.);
#1932=FACE_OUTER_BOUND('',#2843,.T.);
#1933=FACE_OUTER_BOUND('',#2844,.T.);
#1934=FACE_OUTER_BOUND('',#2845,.T.);
#1935=FACE_OUTER_BOUND('',#2846,.T.);
#1936=FACE_OUTER_BOUND('',#2847,.T.);
#1937=FACE_OUTER_BOUND('',#2848,.T.);
#1938=FACE_OUTER_BOUND('',#2849,.T.);
#1939=FACE_OUTER_BOUND('',#2850,.T.);
#1940=FACE_OUTER_BOUND('',#2851,.T.);
#1941=FACE_OUTER_BOUND('',#2852,.T.);
#1942=FACE_OUTER_BOUND('',#2853,.T.);
#1943=FACE_OUTER_BOUND('',#2854,.T.);
#1944=FACE_OUTER_BOUND('',#2855,.T.);
#1945=FACE_OUTER_BOUND('',#2856,.T.);
#1946=FACE_OUTER_BOUND('',#2857,.T.);
#1947=FACE_OUTER_BOUND('',#2858,.T.);
#1948=FACE_OUTER_BOUND('',#2859,.T.);
#1949=FACE_OUTER_BOUND('',#2860,.T.);
#1950=FACE_OUTER_BOUND('',#2861,.T.);
#1951=FACE_OUTER_BOUND('',#2862,.T.);
#1952=FACE_OUTER_BOUND('',#2863,.T.);
#1953=FACE_OUTER_BOUND('',#2864,.T.);
#1954=FACE_OUTER_BOUND('',#2865,.T.);
#1955=FACE_OUTER_BOUND('',#2866,.T.);
#1956=FACE_OUTER_BOUND('',#2867,.T.);
#1957=FACE_OUTER_BOUND('',#2868,.T.);
#1958=FACE_OUTER_BOUND('',#2869,.T.);
#1959=FACE_OUTER_BOUND('',#2870,.T.);
#1960=FACE_OUTER_BOUND('',#2871,.T.);
#1961=FACE_OUTER_BOUND('',#2872,.T.);
#1962=FACE_OUTER_BOUND('',#2873,.T.);
#1963=FACE_OUTER_BOUND('',#2874,.T.);
#1964=FACE_OUTER_BOUND('',#2875,.T.);
#1965=FACE_OUTER_BOUND('',#2876,.T.);
#1966=FACE_OUTER_BOUND('',#2877,.T.);
#1967=FACE_OUTER_BOUND('',#2878,.T.);
#1968=FACE_OUTER_BOUND('',#2879,.T.);
#1969=FACE_OUTER_BOUND('',#2880,.T.);
#1970=FACE_OUTER_BOUND('',#2881,.T.);
#1971=FACE_OUTER_BOUND('',#2882,.T.);
#1972=FACE_OUTER_BOUND('',#2883,.T.);
#1973=FACE_OUTER_BOUND('',#2884,.T.);
#1974=FACE_OUTER_BOUND('',#2885,.T.);
#1975=FACE_OUTER_BOUND('',#2886,.T.);
#1976=FACE_OUTER_BOUND('',#2887,.T.);
#1977=FACE_OUTER_BOUND('',#2888,.T.);
#1978=FACE_OUTER_BOUND('',#2889,.T.);
#1979=FACE_OUTER_BOUND('',#2890,.T.);
#1980=FACE_OUTER_BOUND('',#2891,.T.);
#1981=FACE_OUTER_BOUND('',#2892,.T.);
#1982=FACE_OUTER_BOUND('',#2893,.T.);
#1983=FACE_OUTER_BOUND('',#2894,.T.);
#1984=FACE_OUTER_BOUND('',#2895,.T.);
#1985=FACE_OUTER_BOUND('',#2896,.T.);
#1986=FACE_OUTER_BOUND('',#2897,.T.);
#1987=FACE_OUTER_BOUND('',#2898,.T.);
#1988=FACE_OUTER_BOUND('',#2899,.T.);
#1989=FACE_OUTER_BOUND('',#2900,.T.);
#1990=FACE_OUTER_BOUND('',#2901,.T.);
#1991=FACE_OUTER_BOUND('',#2902,.T.);
#1992=FACE_OUTER_BOUND('',#2903,.T.);
#1993=FACE_OUTER_BOUND('',#2904,.T.);
#1994=FACE_OUTER_BOUND('',#2905,.T.);
#1995=FACE_OUTER_BOUND('',#2906,.T.);
#1996=FACE_OUTER_BOUND('',#2907,.T.);
#1997=FACE_OUTER_BOUND('',#2908,.T.);
#1998=FACE_OUTER_BOUND('',#2909,.T.);
#1999=FACE_OUTER_BOUND('',#2910,.T.);
#2000=FACE_OUTER_BOUND('',#2911,.T.);
#2001=FACE_OUTER_BOUND('',#2912,.T.);
#2002=FACE_OUTER_BOUND('',#2913,.T.);
#2003=FACE_OUTER_BOUND('',#2914,.T.);
#2004=FACE_OUTER_BOUND('',#2915,.T.);
#2005=FACE_OUTER_BOUND('',#2916,.T.);
#2006=FACE_OUTER_BOUND('',#2917,.T.);
#2007=FACE_OUTER_BOUND('',#2918,.T.);
#2008=FACE_OUTER_BOUND('',#2919,.T.);
#2009=FACE_OUTER_BOUND('',#2920,.T.);
#2010=FACE_OUTER_BOUND('',#2921,.T.);
#2011=FACE_OUTER_BOUND('',#2922,.T.);
#2012=FACE_OUTER_BOUND('',#2923,.T.);
#2013=FACE_OUTER_BOUND('',#2924,.T.);
#2014=FACE_OUTER_BOUND('',#2925,.T.);
#2015=FACE_OUTER_BOUND('',#2926,.T.);
#2016=FACE_OUTER_BOUND('',#2927,.T.);
#2017=FACE_OUTER_BOUND('',#2928,.T.);
#2018=FACE_OUTER_BOUND('',#2929,.T.);
#2019=FACE_OUTER_BOUND('',#2930,.T.);
#2020=FACE_OUTER_BOUND('',#2931,.T.);
#2021=FACE_OUTER_BOUND('',#2932,.T.);
#2022=FACE_OUTER_BOUND('',#2933,.T.);
#2023=FACE_OUTER_BOUND('',#2934,.T.);
#2024=FACE_OUTER_BOUND('',#2935,.T.);
#2025=FACE_OUTER_BOUND('',#2936,.T.);
#2026=FACE_OUTER_BOUND('',#2937,.T.);
#2027=FACE_OUTER_BOUND('',#2938,.T.);
#2028=FACE_OUTER_BOUND('',#2943,.T.);
#2029=FACE_OUTER_BOUND('',#2944,.T.);
#2030=FACE_OUTER_BOUND('',#2945,.T.);
#2031=FACE_OUTER_BOUND('',#2946,.T.);
#2032=FACE_OUTER_BOUND('',#2947,.T.);
#2033=FACE_OUTER_BOUND('',#2948,.T.);
#2034=FACE_OUTER_BOUND('',#2949,.T.);
#2035=FACE_OUTER_BOUND('',#2950,.T.);
#2036=FACE_OUTER_BOUND('',#2951,.T.);
#2037=FACE_OUTER_BOUND('',#2952,.T.);
#2038=FACE_OUTER_BOUND('',#2953,.T.);
#2039=FACE_OUTER_BOUND('',#2954,.T.);
#2040=FACE_OUTER_BOUND('',#2955,.T.);
#2041=FACE_OUTER_BOUND('',#2956,.T.);
#2042=FACE_OUTER_BOUND('',#2957,.T.);
#2043=FACE_OUTER_BOUND('',#2958,.T.);
#2044=FACE_OUTER_BOUND('',#2959,.T.);
#2045=FACE_OUTER_BOUND('',#2960,.T.);
#2046=FACE_OUTER_BOUND('',#2961,.T.);
#2047=FACE_OUTER_BOUND('',#2962,.T.);
#2048=FACE_OUTER_BOUND('',#2963,.T.);
#2049=FACE_OUTER_BOUND('',#2964,.T.);
#2050=FACE_OUTER_BOUND('',#2965,.T.);
#2051=FACE_OUTER_BOUND('',#2966,.T.);
#2052=FACE_OUTER_BOUND('',#2967,.T.);
#2053=FACE_OUTER_BOUND('',#2968,.T.);
#2054=FACE_OUTER_BOUND('',#2969,.T.);
#2055=FACE_OUTER_BOUND('',#2970,.T.);
#2056=FACE_OUTER_BOUND('',#2971,.T.);
#2057=FACE_OUTER_BOUND('',#2972,.T.);
#2058=FACE_OUTER_BOUND('',#2973,.T.);
#2059=FACE_OUTER_BOUND('',#2974,.T.);
#2060=FACE_OUTER_BOUND('',#2975,.T.);
#2061=FACE_OUTER_BOUND('',#2976,.T.);
#2062=FACE_OUTER_BOUND('',#2977,.T.);
#2063=FACE_OUTER_BOUND('',#2978,.T.);
#2064=FACE_OUTER_BOUND('',#2979,.T.);
#2065=FACE_OUTER_BOUND('',#2980,.T.);
#2066=FACE_OUTER_BOUND('',#2981,.T.);
#2067=FACE_OUTER_BOUND('',#2982,.T.);
#2068=FACE_OUTER_BOUND('',#2983,.T.);
#2069=FACE_OUTER_BOUND('',#2984,.T.);
#2070=FACE_OUTER_BOUND('',#2986,.T.);
#2071=FACE_OUTER_BOUND('',#2987,.T.);
#2072=FACE_OUTER_BOUND('',#2988,.T.);
#2073=FACE_OUTER_BOUND('',#2989,.T.);
#2074=FACE_OUTER_BOUND('',#2990,.T.);
#2075=FACE_OUTER_BOUND('',#2991,.T.);
#2076=FACE_OUTER_BOUND('',#2992,.T.);
#2077=FACE_OUTER_BOUND('',#2993,.T.);
#2078=FACE_OUTER_BOUND('',#2994,.T.);
#2079=FACE_OUTER_BOUND('',#2995,.T.);
#2080=FACE_OUTER_BOUND('',#2996,.T.);
#2081=FACE_OUTER_BOUND('',#2997,.T.);
#2082=FACE_OUTER_BOUND('',#2998,.T.);
#2083=FACE_OUTER_BOUND('',#2999,.T.);
#2084=FACE_OUTER_BOUND('',#3000,.T.);
#2085=FACE_OUTER_BOUND('',#3001,.T.);
#2086=FACE_OUTER_BOUND('',#3002,.T.);
#2087=FACE_OUTER_BOUND('',#3004,.T.);
#2088=FACE_OUTER_BOUND('',#3006,.T.);
#2089=FACE_OUTER_BOUND('',#3007,.T.);
#2090=FACE_OUTER_BOUND('',#3008,.T.);
#2091=FACE_OUTER_BOUND('',#3011,.T.);
#2092=FACE_OUTER_BOUND('',#3013,.T.);
#2093=FACE_OUTER_BOUND('',#3015,.T.);
#2094=FACE_OUTER_BOUND('',#3016,.T.);
#2095=FACE_OUTER_BOUND('',#3017,.T.);
#2096=FACE_OUTER_BOUND('',#3019,.T.);
#2097=FACE_OUTER_BOUND('',#3021,.T.);
#2098=FACE_OUTER_BOUND('',#3022,.T.);
#2099=FACE_OUTER_BOUND('',#3023,.T.);
#2100=FACE_OUTER_BOUND('',#3025,.T.);
#2101=FACE_OUTER_BOUND('',#3027,.T.);
#2102=FACE_OUTER_BOUND('',#3028,.T.);
#2103=FACE_OUTER_BOUND('',#3029,.T.);
#2104=FACE_OUTER_BOUND('',#3031,.T.);
#2105=FACE_OUTER_BOUND('',#3033,.T.);
#2106=FACE_OUTER_BOUND('',#3034,.T.);
#2107=FACE_OUTER_BOUND('',#3035,.T.);
#2108=FACE_OUTER_BOUND('',#3037,.T.);
#2109=FACE_OUTER_BOUND('',#3039,.T.);
#2110=FACE_OUTER_BOUND('',#3040,.T.);
#2111=FACE_OUTER_BOUND('',#3041,.T.);
#2112=FACE_OUTER_BOUND('',#3043,.T.);
#2113=FACE_OUTER_BOUND('',#3045,.T.);
#2114=FACE_OUTER_BOUND('',#3046,.T.);
#2115=FACE_OUTER_BOUND('',#3047,.T.);
#2116=FACE_OUTER_BOUND('',#3049,.T.);
#2117=FACE_OUTER_BOUND('',#3051,.T.);
#2118=FACE_OUTER_BOUND('',#3052,.T.);
#2119=FACE_OUTER_BOUND('',#3053,.T.);
#2120=FACE_OUTER_BOUND('',#3054,.T.);
#2121=FACE_OUTER_BOUND('',#3055,.T.);
#2122=FACE_OUTER_BOUND('',#3057,.T.);
#2123=FACE_OUTER_BOUND('',#3058,.T.);
#2124=FACE_OUTER_BOUND('',#3059,.T.);
#2125=FACE_OUTER_BOUND('',#3060,.T.);
#2126=FACE_OUTER_BOUND('',#3062,.T.);
#2127=FACE_OUTER_BOUND('',#3063,.T.);
#2128=FACE_OUTER_BOUND('',#3065,.T.);
#2129=FACE_OUTER_BOUND('',#3067,.T.);
#2130=FACE_OUTER_BOUND('',#3069,.T.);
#2131=FACE_OUTER_BOUND('',#3070,.T.);
#2132=FACE_OUTER_BOUND('',#3071,.T.);
#2133=FACE_OUTER_BOUND('',#3073,.T.);
#2134=FACE_OUTER_BOUND('',#3075,.T.);
#2135=FACE_OUTER_BOUND('',#3076,.T.);
#2136=FACE_OUTER_BOUND('',#3077,.T.);
#2137=FACE_OUTER_BOUND('',#3078,.T.);
#2138=FACE_OUTER_BOUND('',#3080,.T.);
#2139=FACE_OUTER_BOUND('',#3081,.T.);
#2140=FACE_OUTER_BOUND('',#3082,.T.);
#2141=FACE_OUTER_BOUND('',#3084,.T.);
#2142=FACE_OUTER_BOUND('',#3085,.T.);
#2143=FACE_OUTER_BOUND('',#3086,.T.);
#2144=FACE_OUTER_BOUND('',#3087,.T.);
#2145=FACE_OUTER_BOUND('',#3088,.T.);
#2146=FACE_OUTER_BOUND('',#3089,.T.);
#2147=FACE_OUTER_BOUND('',#3090,.T.);
#2148=FACE_OUTER_BOUND('',#3091,.T.);
#2149=FACE_OUTER_BOUND('',#3092,.T.);
#2150=FACE_OUTER_BOUND('',#3093,.T.);
#2151=FACE_OUTER_BOUND('',#3094,.T.);
#2152=FACE_OUTER_BOUND('',#3095,.T.);
#2153=FACE_OUTER_BOUND('',#3096,.T.);
#2154=FACE_OUTER_BOUND('',#3097,.T.);
#2155=FACE_OUTER_BOUND('',#3098,.T.);
#2156=FACE_OUTER_BOUND('',#3099,.T.);
#2157=FACE_OUTER_BOUND('',#3100,.T.);
#2158=FACE_OUTER_BOUND('',#3101,.T.);
#2159=FACE_OUTER_BOUND('',#3102,.T.);
#2160=FACE_OUTER_BOUND('',#3103,.T.);
#2161=FACE_OUTER_BOUND('',#3104,.T.);
#2162=FACE_OUTER_BOUND('',#3105,.T.);
#2163=FACE_OUTER_BOUND('',#3106,.T.);
#2164=FACE_OUTER_BOUND('',#3107,.T.);
#2165=FACE_OUTER_BOUND('',#3108,.T.);
#2166=FACE_OUTER_BOUND('',#3109,.T.);
#2167=FACE_OUTER_BOUND('',#3110,.T.);
#2168=FACE_OUTER_BOUND('',#3111,.T.);
#2169=FACE_OUTER_BOUND('',#3112,.T.);
#2170=FACE_OUTER_BOUND('',#3113,.T.);
#2171=FACE_OUTER_BOUND('',#3114,.T.);
#2172=FACE_OUTER_BOUND('',#3115,.T.);
#2173=FACE_OUTER_BOUND('',#3116,.T.);
#2174=FACE_OUTER_BOUND('',#3117,.T.);
#2175=FACE_OUTER_BOUND('',#3118,.T.);
#2176=FACE_OUTER_BOUND('',#3119,.T.);
#2177=FACE_OUTER_BOUND('',#3120,.T.);
#2178=FACE_OUTER_BOUND('',#3121,.T.);
#2179=FACE_OUTER_BOUND('',#3122,.T.);
#2180=FACE_OUTER_BOUND('',#3123,.T.);
#2181=FACE_OUTER_BOUND('',#3124,.T.);
#2182=FACE_OUTER_BOUND('',#3125,.T.);
#2183=FACE_OUTER_BOUND('',#3126,.T.);
#2184=FACE_OUTER_BOUND('',#3127,.T.);
#2185=FACE_OUTER_BOUND('',#3128,.T.);
#2186=FACE_OUTER_BOUND('',#3129,.T.);
#2187=FACE_OUTER_BOUND('',#3130,.T.);
#2188=FACE_OUTER_BOUND('',#3131,.T.);
#2189=FACE_OUTER_BOUND('',#3132,.T.);
#2190=FACE_OUTER_BOUND('',#3133,.T.);
#2191=FACE_OUTER_BOUND('',#3134,.T.);
#2192=FACE_OUTER_BOUND('',#3135,.T.);
#2193=FACE_OUTER_BOUND('',#3136,.T.);
#2194=FACE_OUTER_BOUND('',#3137,.T.);
#2195=FACE_OUTER_BOUND('',#3138,.T.);
#2196=FACE_OUTER_BOUND('',#3139,.T.);
#2197=FACE_OUTER_BOUND('',#3140,.T.);
#2198=FACE_OUTER_BOUND('',#3141,.T.);
#2199=FACE_OUTER_BOUND('',#3142,.T.);
#2200=FACE_OUTER_BOUND('',#3143,.T.);
#2201=FACE_OUTER_BOUND('',#3144,.T.);
#2202=FACE_OUTER_BOUND('',#3145,.T.);
#2203=FACE_OUTER_BOUND('',#3146,.T.);
#2204=FACE_OUTER_BOUND('',#3147,.T.);
#2205=FACE_OUTER_BOUND('',#3148,.T.);
#2206=FACE_OUTER_BOUND('',#3149,.T.);
#2207=FACE_OUTER_BOUND('',#3150,.T.);
#2208=FACE_OUTER_BOUND('',#3151,.T.);
#2209=FACE_OUTER_BOUND('',#3152,.T.);
#2210=FACE_OUTER_BOUND('',#3153,.T.);
#2211=FACE_OUTER_BOUND('',#3154,.T.);
#2212=FACE_OUTER_BOUND('',#3155,.T.);
#2213=FACE_OUTER_BOUND('',#3156,.T.);
#2214=FACE_OUTER_BOUND('',#3157,.T.);
#2215=FACE_OUTER_BOUND('',#3158,.T.);
#2216=FACE_OUTER_BOUND('',#3159,.T.);
#2217=FACE_OUTER_BOUND('',#3160,.T.);
#2218=FACE_OUTER_BOUND('',#3161,.T.);
#2219=FACE_OUTER_BOUND('',#3162,.T.);
#2220=FACE_OUTER_BOUND('',#3163,.T.);
#2221=FACE_OUTER_BOUND('',#3165,.T.);
#2222=FACE_OUTER_BOUND('',#3166,.T.);
#2223=FACE_OUTER_BOUND('',#3167,.T.);
#2224=FACE_OUTER_BOUND('',#3168,.T.);
#2225=FACE_OUTER_BOUND('',#3169,.T.);
#2226=FACE_OUTER_BOUND('',#3170,.T.);
#2227=FACE_OUTER_BOUND('',#3172,.T.);
#2228=FACE_OUTER_BOUND('',#3173,.T.);
#2229=FACE_OUTER_BOUND('',#3174,.T.);
#2230=FACE_OUTER_BOUND('',#3175,.T.);
#2231=FACE_OUTER_BOUND('',#3176,.T.);
#2232=FACE_OUTER_BOUND('',#3177,.T.);
#2233=FACE_OUTER_BOUND('',#3178,.T.);
#2234=FACE_OUTER_BOUND('',#3179,.T.);
#2235=FACE_OUTER_BOUND('',#3180,.T.);
#2236=FACE_OUTER_BOUND('',#3181,.T.);
#2237=FACE_OUTER_BOUND('',#3182,.T.);
#2238=FACE_OUTER_BOUND('',#3183,.T.);
#2239=FACE_OUTER_BOUND('',#3184,.T.);
#2240=FACE_OUTER_BOUND('',#3185,.T.);
#2241=FACE_OUTER_BOUND('',#3186,.T.);
#2242=FACE_OUTER_BOUND('',#3187,.T.);
#2243=FACE_OUTER_BOUND('',#3188,.T.);
#2244=FACE_OUTER_BOUND('',#3189,.T.);
#2245=FACE_OUTER_BOUND('',#3190,.T.);
#2246=FACE_OUTER_BOUND('',#3191,.T.);
#2247=FACE_OUTER_BOUND('',#3192,.T.);
#2248=FACE_OUTER_BOUND('',#3193,.T.);
#2249=FACE_OUTER_BOUND('',#3194,.T.);
#2250=FACE_OUTER_BOUND('',#3195,.T.);
#2251=FACE_OUTER_BOUND('',#3196,.T.);
#2252=FACE_OUTER_BOUND('',#3198,.T.);
#2253=FACE_OUTER_BOUND('',#3200,.T.);
#2254=FACE_OUTER_BOUND('',#3201,.T.);
#2255=FACE_OUTER_BOUND('',#3202,.T.);
#2256=FACE_OUTER_BOUND('',#3203,.T.);
#2257=FACE_OUTER_BOUND('',#3204,.T.);
#2258=FACE_OUTER_BOUND('',#3206,.T.);
#2259=FACE_OUTER_BOUND('',#3207,.T.);
#2260=FACE_OUTER_BOUND('',#3208,.T.);
#2261=FACE_OUTER_BOUND('',#3209,.T.);
#2262=FACE_OUTER_BOUND('',#3210,.T.);
#2263=FACE_OUTER_BOUND('',#3211,.T.);
#2264=FACE_OUTER_BOUND('',#3212,.T.);
#2265=FACE_OUTER_BOUND('',#3213,.T.);
#2266=FACE_OUTER_BOUND('',#3214,.T.);
#2267=FACE_OUTER_BOUND('',#3215,.T.);
#2268=FACE_OUTER_BOUND('',#3216,.T.);
#2269=FACE_OUTER_BOUND('',#3217,.T.);
#2270=FACE_OUTER_BOUND('',#3218,.T.);
#2271=FACE_OUTER_BOUND('',#3219,.T.);
#2272=FACE_OUTER_BOUND('',#3220,.T.);
#2273=FACE_OUTER_BOUND('',#3222,.T.);
#2274=EDGE_LOOP('',(#9234,#9235,#9236,#9237));
#2275=EDGE_LOOP('',(#9238,#9239,#9240,#9241));
#2276=EDGE_LOOP('',(#9242,#9243,#9244,#9245));
#2277=EDGE_LOOP('',(#9246,#9247,#9248,#9249));
#2278=EDGE_LOOP('',(#9250,#9251,#9252,#9253));
#2279=EDGE_LOOP('',(#9254,#9255,#9256,#9257));
#2280=EDGE_LOOP('',(#9258,#9259,#9260,#9261));
#2281=EDGE_LOOP('',(#9262,#9263,#9264,#9265));
#2282=EDGE_LOOP('',(#9266,#9267,#9268,#9269));
#2283=EDGE_LOOP('',(#9270));
#2284=EDGE_LOOP('',(#9271));
#2285=EDGE_LOOP('',(#9272));
#2286=EDGE_LOOP('',(#9273));
#2287=EDGE_LOOP('',(#9274,#9275,#9276,#9277));
#2288=EDGE_LOOP('',(#9278));
#2289=EDGE_LOOP('',(#9279));
#2290=EDGE_LOOP('',(#9280));
#2291=EDGE_LOOP('',(#9281));
#2292=EDGE_LOOP('',(#9282,#9283,#9284,#9285));
#2293=EDGE_LOOP('',(#9286,#9287,#9288,#9289));
#2294=EDGE_LOOP('',(#9290,#9291,#9292,#9293));
#2295=EDGE_LOOP('',(#9294,#9295,#9296,#9297));
#2296=EDGE_LOOP('',(#9298,#9299,#9300,#9301));
#2297=EDGE_LOOP('',(#9302,#9303,#9304,#9305));
#2298=EDGE_LOOP('',(#9306,#9307,#9308,#9309));
#2299=EDGE_LOOP('',(#9310,#9311,#9312,#9313));
#2300=EDGE_LOOP('',(#9314,#9315,#9316,#9317));
#2301=EDGE_LOOP('',(#9318,#9319,#9320,#9321));
#2302=EDGE_LOOP('',(#9322,#9323,#9324,#9325));
#2303=EDGE_LOOP('',(#9326,#9327,#9328,#9329));
#2304=EDGE_LOOP('',(#9330,#9331,#9332,#9333));
#2305=EDGE_LOOP('',(#9334,#9335,#9336,#9337));
#2306=EDGE_LOOP('',(#9338,#9339,#9340,#9341));
#2307=EDGE_LOOP('',(#9342,#9343,#9344,#9345));
#2308=EDGE_LOOP('',(#9346,#9347,#9348,#9349));
#2309=EDGE_LOOP('',(#9350,#9351,#9352,#9353));
#2310=EDGE_LOOP('',(#9354,#9355,#9356,#9357));
#2311=EDGE_LOOP('',(#9358,#9359,#9360,#9361));
#2312=EDGE_LOOP('',(#9362,#9363,#9364,#9365));
#2313=EDGE_LOOP('',(#9366,#9367,#9368,#9369));
#2314=EDGE_LOOP('',(#9370,#9371,#9372,#9373));
#2315=EDGE_LOOP('',(#9374,#9375,#9376,#9377));
#2316=EDGE_LOOP('',(#9378,#9379,#9380,#9381));
#2317=EDGE_LOOP('',(#9382,#9383,#9384,#9385));
#2318=EDGE_LOOP('',(#9386,#9387,#9388,#9389));
#2319=EDGE_LOOP('',(#9390,#9391,#9392,#9393));
#2320=EDGE_LOOP('',(#9394,#9395,#9396,#9397));
#2321=EDGE_LOOP('',(#9398,#9399,#9400,#9401));
#2322=EDGE_LOOP('',(#9402,#9403,#9404,#9405));
#2323=EDGE_LOOP('',(#9406,#9407,#9408,#9409));
#2324=EDGE_LOOP('',(#9410,#9411,#9412,#9413));
#2325=EDGE_LOOP('',(#9414));
#2326=EDGE_LOOP('',(#9415));
#2327=EDGE_LOOP('',(#9416));
#2328=EDGE_LOOP('',(#9417));
#2329=EDGE_LOOP('',(#9418));
#2330=EDGE_LOOP('',(#9419));
#2331=EDGE_LOOP('',(#9420));
#2332=EDGE_LOOP('',(#9421));
#2333=EDGE_LOOP('',(#9422));
#2334=EDGE_LOOP('',(#9423));
#2335=EDGE_LOOP('',(#9424));
#2336=EDGE_LOOP('',(#9425));
#2337=EDGE_LOOP('',(#9426));
#2338=EDGE_LOOP('',(#9427));
#2339=EDGE_LOOP('',(#9428));
#2340=EDGE_LOOP('',(#9429));
#2341=EDGE_LOOP('',(#9430,#9431,#9432,#9433));
#2342=EDGE_LOOP('',(#9434));
#2343=EDGE_LOOP('',(#9435));
#2344=EDGE_LOOP('',(#9436));
#2345=EDGE_LOOP('',(#9437));
#2346=EDGE_LOOP('',(#9438));
#2347=EDGE_LOOP('',(#9439));
#2348=EDGE_LOOP('',(#9440));
#2349=EDGE_LOOP('',(#9441));
#2350=EDGE_LOOP('',(#9442));
#2351=EDGE_LOOP('',(#9443));
#2352=EDGE_LOOP('',(#9444));
#2353=EDGE_LOOP('',(#9445));
#2354=EDGE_LOOP('',(#9446));
#2355=EDGE_LOOP('',(#9447));
#2356=EDGE_LOOP('',(#9448));
#2357=EDGE_LOOP('',(#9449));
#2358=EDGE_LOOP('',(#9450,#9451,#9452,#9453));
#2359=EDGE_LOOP('',(#9454));
#2360=EDGE_LOOP('',(#9455));
#2361=EDGE_LOOP('',(#9456,#9457,#9458,#9459));
#2362=EDGE_LOOP('',(#9460));
#2363=EDGE_LOOP('',(#9461));
#2364=EDGE_LOOP('',(#9462,#9463,#9464,#9465));
#2365=EDGE_LOOP('',(#9466,#9467,#9468,#9469));
#2366=EDGE_LOOP('',(#9470,#9471,#9472,#9473));
#2367=EDGE_LOOP('',(#9474,#9475,#9476,#9477));
#2368=EDGE_LOOP('',(#9478,#9479,#9480,#9481));
#2369=EDGE_LOOP('',(#9482,#9483,#9484,#9485));
#2370=EDGE_LOOP('',(#9486,#9487,#9488,#9489));
#2371=EDGE_LOOP('',(#9490));
#2372=EDGE_LOOP('',(#9491));
#2373=EDGE_LOOP('',(#9492,#9493,#9494,#9495));
#2374=EDGE_LOOP('',(#9496));
#2375=EDGE_LOOP('',(#9497));
#2376=EDGE_LOOP('',(#9498,#9499,#9500,#9501));
#2377=EDGE_LOOP('',(#9502,#9503,#9504,#9505));
#2378=EDGE_LOOP('',(#9506,#9507,#9508,#9509));
#2379=EDGE_LOOP('',(#9510,#9511,#9512,#9513));
#2380=EDGE_LOOP('',(#9514,#9515,#9516,#9517));
#2381=EDGE_LOOP('',(#9518,#9519,#9520,#9521));
#2382=EDGE_LOOP('',(#9522,#9523,#9524,#9525));
#2383=EDGE_LOOP('',(#9526));
#2384=EDGE_LOOP('',(#9527));
#2385=EDGE_LOOP('',(#9528,#9529,#9530,#9531));
#2386=EDGE_LOOP('',(#9532));
#2387=EDGE_LOOP('',(#9533));
#2388=EDGE_LOOP('',(#9534,#9535,#9536,#9537));
#2389=EDGE_LOOP('',(#9538,#9539,#9540,#9541));
#2390=EDGE_LOOP('',(#9542,#9543,#9544,#9545));
#2391=EDGE_LOOP('',(#9546,#9547,#9548,#9549));
#2392=EDGE_LOOP('',(#9550,#9551,#9552,#9553));
#2393=EDGE_LOOP('',(#9554,#9555,#9556,#9557));
#2394=EDGE_LOOP('',(#9558,#9559,#9560,#9561));
#2395=EDGE_LOOP('',(#9562));
#2396=EDGE_LOOP('',(#9563));
#2397=EDGE_LOOP('',(#9564,#9565,#9566,#9567));
#2398=EDGE_LOOP('',(#9568));
#2399=EDGE_LOOP('',(#9569));
#2400=EDGE_LOOP('',(#9570,#9571,#9572,#9573));
#2401=EDGE_LOOP('',(#9574,#9575,#9576,#9577));
#2402=EDGE_LOOP('',(#9578,#9579,#9580,#9581));
#2403=EDGE_LOOP('',(#9582,#9583,#9584,#9585));
#2404=EDGE_LOOP('',(#9586,#9587,#9588,#9589));
#2405=EDGE_LOOP('',(#9590,#9591,#9592,#9593));
#2406=EDGE_LOOP('',(#9594,#9595,#9596,#9597));
#2407=EDGE_LOOP('',(#9598,#9599,#9600,#9601));
#2408=EDGE_LOOP('',(#9602,#9603,#9604,#9605));
#2409=EDGE_LOOP('',(#9606,#9607,#9608,#9609));
#2410=EDGE_LOOP('',(#9610,#9611,#9612,#9613));
#2411=EDGE_LOOP('',(#9614,#9615,#9616,#9617));
#2412=EDGE_LOOP('',(#9618,#9619,#9620,#9621));
#2413=EDGE_LOOP('',(#9622,#9623,#9624,#9625));
#2414=EDGE_LOOP('',(#9626));
#2415=EDGE_LOOP('',(#9627,#9628,#9629,#9630));
#2416=EDGE_LOOP('',(#9631));
#2417=EDGE_LOOP('',(#9632,#9633,#9634,#9635));
#2418=EDGE_LOOP('',(#9636,#9637,#9638,#9639));
#2419=EDGE_LOOP('',(#9640,#9641,#9642,#9643,#9644,#9645,#9646,#9647));
#2420=EDGE_LOOP('',(#9648));
#2421=EDGE_LOOP('',(#9649));
#2422=EDGE_LOOP('',(#9650));
#2423=EDGE_LOOP('',(#9651));
#2424=EDGE_LOOP('',(#9652));
#2425=EDGE_LOOP('',(#9653,#9654,#9655,#9656));
#2426=EDGE_LOOP('',(#9657,#9658,#9659,#9660,#9661,#9662,#9663,#9664));
#2427=EDGE_LOOP('',(#9665));
#2428=EDGE_LOOP('',(#9666));
#2429=EDGE_LOOP('',(#9667));
#2430=EDGE_LOOP('',(#9668));
#2431=EDGE_LOOP('',(#9669));
#2432=EDGE_LOOP('',(#9670,#9671,#9672,#9673));
#2433=EDGE_LOOP('',(#9674,#9675,#9676,#9677));
#2434=EDGE_LOOP('',(#9678,#9679,#9680,#9681));
#2435=EDGE_LOOP('',(#9682));
#2436=EDGE_LOOP('',(#9683));
#2437=EDGE_LOOP('',(#9684,#9685,#9686,#9687));
#2438=EDGE_LOOP('',(#9688,#9689,#9690,#9691));
#2439=EDGE_LOOP('',(#9692,#9693,#9694,#9695));
#2440=EDGE_LOOP('',(#9696,#9697,#9698,#9699));
#2441=EDGE_LOOP('',(#9700,#9701,#9702,#9703));
#2442=EDGE_LOOP('',(#9704));
#2443=EDGE_LOOP('',(#9705));
#2444=EDGE_LOOP('',(#9706,#9707,#9708,#9709));
#2445=EDGE_LOOP('',(#9710,#9711,#9712,#9713));
#2446=EDGE_LOOP('',(#9714));
#2447=EDGE_LOOP('',(#9715));
#2448=EDGE_LOOP('',(#9716));
#2449=EDGE_LOOP('',(#9717));
#2450=EDGE_LOOP('',(#9718));
#2451=EDGE_LOOP('',(#9719));
#2452=EDGE_LOOP('',(#9720));
#2453=EDGE_LOOP('',(#9721));
#2454=EDGE_LOOP('',(#9722));
#2455=EDGE_LOOP('',(#9723));
#2456=EDGE_LOOP('',(#9724));
#2457=EDGE_LOOP('',(#9725));
#2458=EDGE_LOOP('',(#9726,#9727,#9728,#9729));
#2459=EDGE_LOOP('',(#9730,#9731,#9732,#9733));
#2460=EDGE_LOOP('',(#9734,#9735,#9736,#9737));
#2461=EDGE_LOOP('',(#9738,#9739,#9740,#9741));
#2462=EDGE_LOOP('',(#9742,#9743,#9744,#9745));
#2463=EDGE_LOOP('',(#9746));
#2464=EDGE_LOOP('',(#9747));
#2465=EDGE_LOOP('',(#9748,#9749,#9750,#9751));
#2466=EDGE_LOOP('',(#9752,#9753,#9754,#9755));
#2467=EDGE_LOOP('',(#9756));
#2468=EDGE_LOOP('',(#9757));
#2469=EDGE_LOOP('',(#9758));
#2470=EDGE_LOOP('',(#9759));
#2471=EDGE_LOOP('',(#9760));
#2472=EDGE_LOOP('',(#9761));
#2473=EDGE_LOOP('',(#9762));
#2474=EDGE_LOOP('',(#9763));
#2475=EDGE_LOOP('',(#9764));
#2476=EDGE_LOOP('',(#9765));
#2477=EDGE_LOOP('',(#9766));
#2478=EDGE_LOOP('',(#9767));
#2479=EDGE_LOOP('',(#9768,#9769,#9770,#9771));
#2480=EDGE_LOOP('',(#9772,#9773,#9774,#9775));
#2481=EDGE_LOOP('',(#9776,#9777,#9778,#9779));
#2482=EDGE_LOOP('',(#9780,#9781,#9782,#9783));
#2483=EDGE_LOOP('',(#9784,#9785,#9786,#9787));
#2484=EDGE_LOOP('',(#9788,#9789,#9790,#9791));
#2485=EDGE_LOOP('',(#9792,#9793,#9794,#9795));
#2486=EDGE_LOOP('',(#9796,#9797,#9798,#9799));
#2487=EDGE_LOOP('',(#9800));
#2488=EDGE_LOOP('',(#9801,#9802,#9803,#9804));
#2489=EDGE_LOOP('',(#9805));
#2490=EDGE_LOOP('',(#9806,#9807,#9808,#9809));
#2491=EDGE_LOOP('',(#9810,#9811,#9812,#9813));
#2492=EDGE_LOOP('',(#9814,#9815,#9816,#9817,#9818,#9819,#9820,#9821));
#2493=EDGE_LOOP('',(#9822));
#2494=EDGE_LOOP('',(#9823));
#2495=EDGE_LOOP('',(#9824));
#2496=EDGE_LOOP('',(#9825));
#2497=EDGE_LOOP('',(#9826));
#2498=EDGE_LOOP('',(#9827,#9828,#9829,#9830));
#2499=EDGE_LOOP('',(#9831,#9832,#9833,#9834,#9835,#9836,#9837,#9838));
#2500=EDGE_LOOP('',(#9839));
#2501=EDGE_LOOP('',(#9840));
#2502=EDGE_LOOP('',(#9841));
#2503=EDGE_LOOP('',(#9842));
#2504=EDGE_LOOP('',(#9843));
#2505=EDGE_LOOP('',(#9844,#9845,#9846,#9847));
#2506=EDGE_LOOP('',(#9848,#9849,#9850,#9851));
#2507=EDGE_LOOP('',(#9852,#9853,#9854,#9855));
#2508=EDGE_LOOP('',(#9856));
#2509=EDGE_LOOP('',(#9857));
#2510=EDGE_LOOP('',(#9858,#9859,#9860,#9861));
#2511=EDGE_LOOP('',(#9862,#9863,#9864,#9865));
#2512=EDGE_LOOP('',(#9866,#9867,#9868,#9869));
#2513=EDGE_LOOP('',(#9870,#9871,#9872,#9873));
#2514=EDGE_LOOP('',(#9874,#9875,#9876,#9877));
#2515=EDGE_LOOP('',(#9878));
#2516=EDGE_LOOP('',(#9879));
#2517=EDGE_LOOP('',(#9880,#9881,#9882,#9883));
#2518=EDGE_LOOP('',(#9884,#9885,#9886,#9887));
#2519=EDGE_LOOP('',(#9888));
#2520=EDGE_LOOP('',(#9889));
#2521=EDGE_LOOP('',(#9890));
#2522=EDGE_LOOP('',(#9891));
#2523=EDGE_LOOP('',(#9892));
#2524=EDGE_LOOP('',(#9893));
#2525=EDGE_LOOP('',(#9894));
#2526=EDGE_LOOP('',(#9895));
#2527=EDGE_LOOP('',(#9896));
#2528=EDGE_LOOP('',(#9897));
#2529=EDGE_LOOP('',(#9898));
#2530=EDGE_LOOP('',(#9899));
#2531=EDGE_LOOP('',(#9900,#9901,#9902,#9903));
#2532=EDGE_LOOP('',(#9904,#9905,#9906,#9907));
#2533=EDGE_LOOP('',(#9908,#9909,#9910,#9911));
#2534=EDGE_LOOP('',(#9912,#9913,#9914,#9915));
#2535=EDGE_LOOP('',(#9916,#9917,#9918,#9919));
#2536=EDGE_LOOP('',(#9920));
#2537=EDGE_LOOP('',(#9921));
#2538=EDGE_LOOP('',(#9922,#9923,#9924,#9925));
#2539=EDGE_LOOP('',(#9926,#9927,#9928,#9929));
#2540=EDGE_LOOP('',(#9930));
#2541=EDGE_LOOP('',(#9931));
#2542=EDGE_LOOP('',(#9932));
#2543=EDGE_LOOP('',(#9933));
#2544=EDGE_LOOP('',(#9934));
#2545=EDGE_LOOP('',(#9935));
#2546=EDGE_LOOP('',(#9936));
#2547=EDGE_LOOP('',(#9937));
#2548=EDGE_LOOP('',(#9938));
#2549=EDGE_LOOP('',(#9939));
#2550=EDGE_LOOP('',(#9940));
#2551=EDGE_LOOP('',(#9941));
#2552=EDGE_LOOP('',(#9942,#9943,#9944,#9945));
#2553=EDGE_LOOP('',(#9946,#9947,#9948,#9949));
#2554=EDGE_LOOP('',(#9950,#9951,#9952,#9953));
#2555=EDGE_LOOP('',(#9954,#9955,#9956,#9957));
#2556=EDGE_LOOP('',(#9958,#9959,#9960,#9961));
#2557=EDGE_LOOP('',(#9962,#9963,#9964,#9965));
#2558=EDGE_LOOP('',(#9966,#9967,#9968,#9969));
#2559=EDGE_LOOP('',(#9970,#9971,#9972,#9973));
#2560=EDGE_LOOP('',(#9974,#9975,#9976,#9977));
#2561=EDGE_LOOP('',(#9978,#9979,#9980,#9981));
#2562=EDGE_LOOP('',(#9982,#9983,#9984,#9985));
#2563=EDGE_LOOP('',(#9986,#9987,#9988,#9989));
#2564=EDGE_LOOP('',(#9990,#9991,#9992,#9993));
#2565=EDGE_LOOP('',(#9994,#9995,#9996,#9997));
#2566=EDGE_LOOP('',(#9998,#9999,#10000,#10001));
#2567=EDGE_LOOP('',(#10002,#10003,#10004,#10005));
#2568=EDGE_LOOP('',(#10006,#10007,#10008,#10009));
#2569=EDGE_LOOP('',(#10010,#10011,#10012,#10013));
#2570=EDGE_LOOP('',(#10014,#10015,#10016,#10017));
#2571=EDGE_LOOP('',(#10018,#10019,#10020,#10021));
#2572=EDGE_LOOP('',(#10022,#10023,#10024,#10025));
#2573=EDGE_LOOP('',(#10026,#10027,#10028,#10029));
#2574=EDGE_LOOP('',(#10030,#10031,#10032,#10033));
#2575=EDGE_LOOP('',(#10034,#10035,#10036,#10037));
#2576=EDGE_LOOP('',(#10038,#10039,#10040,#10041));
#2577=EDGE_LOOP('',(#10042,#10043,#10044,#10045));
#2578=EDGE_LOOP('',(#10046,#10047,#10048,#10049));
#2579=EDGE_LOOP('',(#10050,#10051,#10052,#10053));
#2580=EDGE_LOOP('',(#10054,#10055,#10056,#10057));
#2581=EDGE_LOOP('',(#10058,#10059,#10060,#10061));
#2582=EDGE_LOOP('',(#10062,#10063,#10064,#10065));
#2583=EDGE_LOOP('',(#10066,#10067,#10068,#10069));
#2584=EDGE_LOOP('',(#10070,#10071,#10072,#10073));
#2585=EDGE_LOOP('',(#10074,#10075,#10076,#10077));
#2586=EDGE_LOOP('',(#10078,#10079,#10080,#10081));
#2587=EDGE_LOOP('',(#10082,#10083,#10084,#10085));
#2588=EDGE_LOOP('',(#10086,#10087,#10088,#10089));
#2589=EDGE_LOOP('',(#10090,#10091,#10092,#10093));
#2590=EDGE_LOOP('',(#10094,#10095,#10096,#10097));
#2591=EDGE_LOOP('',(#10098,#10099,#10100,#10101));
#2592=EDGE_LOOP('',(#10102,#10103,#10104,#10105));
#2593=EDGE_LOOP('',(#10106,#10107,#10108,#10109));
#2594=EDGE_LOOP('',(#10110,#10111,#10112,#10113));
#2595=EDGE_LOOP('',(#10114,#10115,#10116,#10117));
#2596=EDGE_LOOP('',(#10118,#10119,#10120,#10121));
#2597=EDGE_LOOP('',(#10122,#10123,#10124,#10125,#10126,#10127,#10128,#10129,
#10130,#10131,#10132,#10133,#10134,#10135,#10136,#10137,#10138,#10139,#10140,
#10141,#10142,#10143,#10144,#10145,#10146,#10147,#10148,#10149,#10150,#10151,
#10152,#10153,#10154,#10155,#10156,#10157,#10158,#10159,#10160,#10161,#10162,
#10163,#10164,#10165));
#2598=EDGE_LOOP('',(#10166));
#2599=EDGE_LOOP('',(#10167,#10168,#10169,#10170,#10171,#10172,#10173,#10174,
#10175,#10176,#10177,#10178,#10179,#10180,#10181,#10182,#10183,#10184,#10185,
#10186,#10187,#10188,#10189,#10190,#10191,#10192,#10193,#10194,#10195,#10196,
#10197,#10198,#10199,#10200,#10201,#10202,#10203,#10204,#10205,#10206,#10207,
#10208,#10209,#10210));
#2600=EDGE_LOOP('',(#10211));
#2601=EDGE_LOOP('',(#10212,#10213,#10214,#10215));
#2602=EDGE_LOOP('',(#10216,#10217,#10218,#10219));
#2603=EDGE_LOOP('',(#10220,#10221,#10222,#10223));
#2604=EDGE_LOOP('',(#10224));
#2605=EDGE_LOOP('',(#10225,#10226,#10227,#10228,#10229,#10230,#10231,#10232,
#10233,#10234));
#2606=EDGE_LOOP('',(#10235,#10236,#10237,#10238));
#2607=EDGE_LOOP('',(#10239,#10240,#10241,#10242));
#2608=EDGE_LOOP('',(#10243,#10244,#10245,#10246,#10247,#10248,#10249,#10250,
#10251,#10252));
#2609=EDGE_LOOP('',(#10253,#10254,#10255,#10256));
#2610=EDGE_LOOP('',(#10257,#10258,#10259,#10260,#10261,#10262));
#2611=EDGE_LOOP('',(#10263,#10264,#10265,#10266,#10267,#10268,#10269,#10270));
#2612=EDGE_LOOP('',(#10271,#10272,#10273,#10274,#10275));
#2613=EDGE_LOOP('',(#10276,#10277,#10278,#10279));
#2614=EDGE_LOOP('',(#10280,#10281,#10282,#10283,#10284,#10285));
#2615=EDGE_LOOP('',(#10286,#10287,#10288,#10289));
#2616=EDGE_LOOP('',(#10290,#10291,#10292,#10293));
#2617=EDGE_LOOP('',(#10294,#10295,#10296,#10297));
#2618=EDGE_LOOP('',(#10298));
#2619=EDGE_LOOP('',(#10299));
#2620=EDGE_LOOP('',(#10300,#10301,#10302,#10303));
#2621=EDGE_LOOP('',(#10304));
#2622=EDGE_LOOP('',(#10305));
#2623=EDGE_LOOP('',(#10306,#10307,#10308,#10309));
#2624=EDGE_LOOP('',(#10310));
#2625=EDGE_LOOP('',(#10311));
#2626=EDGE_LOOP('',(#10312,#10313,#10314,#10315));
#2627=EDGE_LOOP('',(#10316));
#2628=EDGE_LOOP('',(#10317));
#2629=EDGE_LOOP('',(#10318,#10319,#10320,#10321));
#2630=EDGE_LOOP('',(#10322));
#2631=EDGE_LOOP('',(#10323));
#2632=EDGE_LOOP('',(#10324,#10325,#10326,#10327));
#2633=EDGE_LOOP('',(#10328));
#2634=EDGE_LOOP('',(#10329));
#2635=EDGE_LOOP('',(#10330,#10331,#10332,#10333));
#2636=EDGE_LOOP('',(#10334,#10335,#10336,#10337));
#2637=EDGE_LOOP('',(#10338,#10339,#10340,#10341));
#2638=EDGE_LOOP('',(#10342,#10343,#10344,#10345));
#2639=EDGE_LOOP('',(#10346,#10347,#10348,#10349));
#2640=EDGE_LOOP('',(#10350,#10351,#10352,#10353));
#2641=EDGE_LOOP('',(#10354,#10355,#10356,#10357));
#2642=EDGE_LOOP('',(#10358,#10359,#10360,#10361));
#2643=EDGE_LOOP('',(#10362,#10363,#10364,#10365));
#2644=EDGE_LOOP('',(#10366));
#2645=EDGE_LOOP('',(#10367));
#2646=EDGE_LOOP('',(#10368));
#2647=EDGE_LOOP('',(#10369));
#2648=EDGE_LOOP('',(#10370,#10371,#10372,#10373));
#2649=EDGE_LOOP('',(#10374,#10375,#10376,#10377));
#2650=EDGE_LOOP('',(#10378,#10379,#10380,#10381));
#2651=EDGE_LOOP('',(#10382,#10383,#10384,#10385));
#2652=EDGE_LOOP('',(#10386,#10387,#10388,#10389));
#2653=EDGE_LOOP('',(#10390,#10391,#10392,#10393));
#2654=EDGE_LOOP('',(#10394));
#2655=EDGE_LOOP('',(#10395));
#2656=EDGE_LOOP('',(#10396));
#2657=EDGE_LOOP('',(#10397));
#2658=EDGE_LOOP('',(#10398,#10399,#10400,#10401));
#2659=EDGE_LOOP('',(#10402,#10403,#10404,#10405,#10406,#10407,#10408,#10409,
#10410,#10411,#10412,#10413));
#2660=EDGE_LOOP('',(#10414,#10415,#10416,#10417,#10418,#10419,#10420,#10421,
#10422,#10423,#10424,#10425));
#2661=EDGE_LOOP('',(#10426));
#2662=EDGE_LOOP('',(#10427,#10428,#10429,#10430));
#2663=EDGE_LOOP('',(#10431,#10432,#10433,#10434));
#2664=EDGE_LOOP('',(#10435,#10436,#10437,#10438));
#2665=EDGE_LOOP('',(#10439));
#2666=EDGE_LOOP('',(#10440));
#2667=EDGE_LOOP('',(#10441,#10442,#10443,#10444));
#2668=EDGE_LOOP('',(#10445,#10446,#10447,#10448));
#2669=EDGE_LOOP('',(#10449,#10450,#10451,#10452));
#2670=EDGE_LOOP('',(#10453));
#2671=EDGE_LOOP('',(#10454,#10455,#10456,#10457));
#2672=EDGE_LOOP('',(#10458,#10459,#10460,#10461));
#2673=EDGE_LOOP('',(#10462,#10463,#10464,#10465));
#2674=EDGE_LOOP('',(#10466,#10467,#10468,#10469));
#2675=EDGE_LOOP('',(#10470,#10471,#10472,#10473));
#2676=EDGE_LOOP('',(#10474,#10475,#10476,#10477));
#2677=EDGE_LOOP('',(#10478,#10479,#10480,#10481,#10482,#10483));
#2678=EDGE_LOOP('',(#10484,#10485,#10486,#10487,#10488,#10489));
#2679=EDGE_LOOP('',(#10490,#10491,#10492,#10493,#10494,#10495));
#2680=EDGE_LOOP('',(#10496,#10497,#10498,#10499,#10500));
#2681=EDGE_LOOP('',(#10501,#10502,#10503,#10504));
#2682=EDGE_LOOP('',(#10505,#10506,#10507,#10508));
#2683=EDGE_LOOP('',(#10509));
#2684=EDGE_LOOP('',(#10510));
#2685=EDGE_LOOP('',(#10511,#10512,#10513,#10514,#10515));
#2686=EDGE_LOOP('',(#10516));
#2687=EDGE_LOOP('',(#10517));
#2688=EDGE_LOOP('',(#10518,#10519,#10520,#10521));
#2689=EDGE_LOOP('',(#10522,#10523,#10524,#10525,#10526,#10527));
#2690=EDGE_LOOP('',(#10528,#10529,#10530,#10531,#10532));
#2691=EDGE_LOOP('',(#10533));
#2692=EDGE_LOOP('',(#10534));
#2693=EDGE_LOOP('',(#10535,#10536,#10537,#10538));
#2694=EDGE_LOOP('',(#10539,#10540,#10541,#10542));
#2695=EDGE_LOOP('',(#10543,#10544,#10545,#10546));
#2696=EDGE_LOOP('',(#10547));
#2697=EDGE_LOOP('',(#10548));
#2698=EDGE_LOOP('',(#10549,#10550,#10551,#10552,#10553));
#2699=EDGE_LOOP('',(#10554,#10555));
#2700=EDGE_LOOP('',(#10556,#10557));
#2701=EDGE_LOOP('',(#10558,#10559));
#2702=EDGE_LOOP('',(#10560,#10561));
#2703=EDGE_LOOP('',(#10562,#10563));
#2704=EDGE_LOOP('',(#10564,#10565));
#2705=EDGE_LOOP('',(#10566,#10567));
#2706=EDGE_LOOP('',(#10568,#10569,#10570,#10571));
#2707=EDGE_LOOP('',(#10572,#10573,#10574,#10575,#10576,#10577,#10578,#10579,
#10580,#10581,#10582,#10583,#10584,#10585,#10586,#10587,#10588,#10589));
#2708=EDGE_LOOP('',(#10590,#10591,#10592,#10593));
#2709=EDGE_LOOP('',(#10594,#10595,#10596,#10597));
#2710=EDGE_LOOP('',(#10598,#10599,#10600,#10601));
#2711=EDGE_LOOP('',(#10602,#10603,#10604,#10605));
#2712=EDGE_LOOP('',(#10606,#10607,#10608,#10609,#10610,#10611));
#2713=EDGE_LOOP('',(#10612,#10613,#10614,#10615));
#2714=EDGE_LOOP('',(#10616,#10617,#10618,#10619));
#2715=EDGE_LOOP('',(#10620,#10621,#10622,#10623));
#2716=EDGE_LOOP('',(#10624,#10625,#10626,#10627));
#2717=EDGE_LOOP('',(#10628,#10629,#10630,#10631));
#2718=EDGE_LOOP('',(#10632,#10633,#10634,#10635,#10636,#10637,#10638,#10639,
#10640,#10641,#10642,#10643,#10644,#10645,#10646,#10647,#10648,#10649));
#2719=EDGE_LOOP('',(#10650,#10651,#10652,#10653));
#2720=EDGE_LOOP('',(#10654,#10655,#10656,#10657));
#2721=EDGE_LOOP('',(#10658));
#2722=EDGE_LOOP('',(#10659));
#2723=EDGE_LOOP('',(#10660,#10661,#10662,#10663));
#2724=EDGE_LOOP('',(#10664));
#2725=EDGE_LOOP('',(#10665));
#2726=EDGE_LOOP('',(#10666,#10667,#10668,#10669));
#2727=EDGE_LOOP('',(#10670));
#2728=EDGE_LOOP('',(#10671));
#2729=EDGE_LOOP('',(#10672,#10673,#10674,#10675));
#2730=EDGE_LOOP('',(#10676));
#2731=EDGE_LOOP('',(#10677));
#2732=EDGE_LOOP('',(#10678,#10679,#10680,#10681));
#2733=EDGE_LOOP('',(#10682));
#2734=EDGE_LOOP('',(#10683));
#2735=EDGE_LOOP('',(#10684,#10685,#10686,#10687));
#2736=EDGE_LOOP('',(#10688,#10689,#10690,#10691));
#2737=EDGE_LOOP('',(#10692,#10693,#10694,#10695));
#2738=EDGE_LOOP('',(#10696,#10697,#10698,#10699));
#2739=EDGE_LOOP('',(#10700,#10701,#10702,#10703));
#2740=EDGE_LOOP('',(#10704,#10705,#10706,#10707));
#2741=EDGE_LOOP('',(#10708,#10709,#10710,#10711));
#2742=EDGE_LOOP('',(#10712,#10713,#10714,#10715,#10716,#10717));
#2743=EDGE_LOOP('',(#10718,#10719,#10720,#10721,#10722,#10723));
#2744=EDGE_LOOP('',(#10724));
#2745=EDGE_LOOP('',(#10725));
#2746=EDGE_LOOP('',(#10726,#10727,#10728,#10729));
#2747=EDGE_LOOP('',(#10730,#10731,#10732,#10733));
#2748=EDGE_LOOP('',(#10734,#10735,#10736,#10737));
#2749=EDGE_LOOP('',(#10738));
#2750=EDGE_LOOP('',(#10739));
#2751=EDGE_LOOP('',(#10740,#10741,#10742,#10743));
#2752=EDGE_LOOP('',(#10744,#10745,#10746,#10747));
#2753=EDGE_LOOP('',(#10748,#10749,#10750,#10751));
#2754=EDGE_LOOP('',(#10752,#10753,#10754,#10755));
#2755=EDGE_LOOP('',(#10756,#10757,#10758,#10759));
#2756=EDGE_LOOP('',(#10760,#10761,#10762,#10763));
#2757=EDGE_LOOP('',(#10764,#10765,#10766,#10767));
#2758=EDGE_LOOP('',(#10768,#10769,#10770,#10771));
#2759=EDGE_LOOP('',(#10772,#10773,#10774,#10775));
#2760=EDGE_LOOP('',(#10776,#10777,#10778,#10779));
#2761=EDGE_LOOP('',(#10780,#10781,#10782,#10783));
#2762=EDGE_LOOP('',(#10784,#10785,#10786,#10787));
#2763=EDGE_LOOP('',(#10788,#10789,#10790,#10791));
#2764=EDGE_LOOP('',(#10792,#10793,#10794,#10795));
#2765=EDGE_LOOP('',(#10796,#10797,#10798,#10799));
#2766=EDGE_LOOP('',(#10800));
#2767=EDGE_LOOP('',(#10801));
#2768=EDGE_LOOP('',(#10802));
#2769=EDGE_LOOP('',(#10803));
#2770=EDGE_LOOP('',(#10804));
#2771=EDGE_LOOP('',(#10805));
#2772=EDGE_LOOP('',(#10806));
#2773=EDGE_LOOP('',(#10807));
#2774=EDGE_LOOP('',(#10808,#10809,#10810,#10811));
#2775=EDGE_LOOP('',(#10812));
#2776=EDGE_LOOP('',(#10813));
#2777=EDGE_LOOP('',(#10814));
#2778=EDGE_LOOP('',(#10815));
#2779=EDGE_LOOP('',(#10816));
#2780=EDGE_LOOP('',(#10817));
#2781=EDGE_LOOP('',(#10818));
#2782=EDGE_LOOP('',(#10819));
#2783=EDGE_LOOP('',(#10820,#10821,#10822,#10823));
#2784=EDGE_LOOP('',(#10824));
#2785=EDGE_LOOP('',(#10825,#10826,#10827,#10828));
#2786=EDGE_LOOP('',(#10829));
#2787=EDGE_LOOP('',(#10830,#10831,#10832,#10833));
#2788=EDGE_LOOP('',(#10834));
#2789=EDGE_LOOP('',(#10835,#10836,#10837,#10838));
#2790=EDGE_LOOP('',(#10839));
#2791=EDGE_LOOP('',(#10840,#10841,#10842,#10843));
#2792=EDGE_LOOP('',(#10844,#10845,#10846,#10847));
#2793=EDGE_LOOP('',(#10848));
#2794=EDGE_LOOP('',(#10849));
#2795=EDGE_LOOP('',(#10850));
#2796=EDGE_LOOP('',(#10851));
#2797=EDGE_LOOP('',(#10852,#10853,#10854,#10855));
#2798=EDGE_LOOP('',(#10856,#10857,#10858,#10859));
#2799=EDGE_LOOP('',(#10860,#10861,#10862,#10863));
#2800=EDGE_LOOP('',(#10864,#10865,#10866,#10867));
#2801=EDGE_LOOP('',(#10868,#10869,#10870,#10871));
#2802=EDGE_LOOP('',(#10872,#10873,#10874,#10875));
#2803=EDGE_LOOP('',(#10876,#10877,#10878,#10879));
#2804=EDGE_LOOP('',(#10880,#10881,#10882,#10883));
#2805=EDGE_LOOP('',(#10884,#10885,#10886,#10887));
#2806=EDGE_LOOP('',(#10888,#10889,#10890,#10891));
#2807=EDGE_LOOP('',(#10892,#10893,#10894,#10895));
#2808=EDGE_LOOP('',(#10896,#10897,#10898,#10899));
#2809=EDGE_LOOP('',(#10900,#10901,#10902,#10903));
#2810=EDGE_LOOP('',(#10904,#10905,#10906,#10907));
#2811=EDGE_LOOP('',(#10908,#10909,#10910,#10911));
#2812=EDGE_LOOP('',(#10912,#10913,#10914,#10915));
#2813=EDGE_LOOP('',(#10916,#10917,#10918,#10919));
#2814=EDGE_LOOP('',(#10920,#10921,#10922,#10923));
#2815=EDGE_LOOP('',(#10924,#10925,#10926,#10927));
#2816=EDGE_LOOP('',(#10928,#10929,#10930,#10931));
#2817=EDGE_LOOP('',(#10932,#10933,#10934,#10935));
#2818=EDGE_LOOP('',(#10936,#10937,#10938,#10939));
#2819=EDGE_LOOP('',(#10940,#10941,#10942,#10943));
#2820=EDGE_LOOP('',(#10944,#10945,#10946,#10947));
#2821=EDGE_LOOP('',(#10948,#10949,#10950,#10951));
#2822=EDGE_LOOP('',(#10952,#10953,#10954,#10955));
#2823=EDGE_LOOP('',(#10956,#10957,#10958,#10959));
#2824=EDGE_LOOP('',(#10960,#10961,#10962,#10963));
#2825=EDGE_LOOP('',(#10964,#10965,#10966,#10967));
#2826=EDGE_LOOP('',(#10968,#10969,#10970,#10971));
#2827=EDGE_LOOP('',(#10972,#10973,#10974,#10975));
#2828=EDGE_LOOP('',(#10976,#10977,#10978,#10979));
#2829=EDGE_LOOP('',(#10980,#10981,#10982,#10983));
#2830=EDGE_LOOP('',(#10984,#10985,#10986,#10987));
#2831=EDGE_LOOP('',(#10988,#10989,#10990,#10991));
#2832=EDGE_LOOP('',(#10992,#10993,#10994,#10995));
#2833=EDGE_LOOP('',(#10996,#10997,#10998,#10999));
#2834=EDGE_LOOP('',(#11000,#11001,#11002,#11003));
#2835=EDGE_LOOP('',(#11004,#11005,#11006,#11007));
#2836=EDGE_LOOP('',(#11008,#11009,#11010,#11011));
#2837=EDGE_LOOP('',(#11012,#11013,#11014,#11015));
#2838=EDGE_LOOP('',(#11016,#11017,#11018,#11019));
#2839=EDGE_LOOP('',(#11020,#11021,#11022,#11023));
#2840=EDGE_LOOP('',(#11024,#11025,#11026,#11027));
#2841=EDGE_LOOP('',(#11028,#11029,#11030,#11031));
#2842=EDGE_LOOP('',(#11032,#11033,#11034,#11035));
#2843=EDGE_LOOP('',(#11036,#11037,#11038,#11039));
#2844=EDGE_LOOP('',(#11040,#11041,#11042,#11043));
#2845=EDGE_LOOP('',(#11044,#11045,#11046,#11047));
#2846=EDGE_LOOP('',(#11048,#11049,#11050,#11051));
#2847=EDGE_LOOP('',(#11052,#11053,#11054,#11055));
#2848=EDGE_LOOP('',(#11056,#11057,#11058,#11059));
#2849=EDGE_LOOP('',(#11060,#11061,#11062,#11063));
#2850=EDGE_LOOP('',(#11064,#11065,#11066,#11067));
#2851=EDGE_LOOP('',(#11068,#11069,#11070,#11071));
#2852=EDGE_LOOP('',(#11072,#11073,#11074,#11075));
#2853=EDGE_LOOP('',(#11076,#11077,#11078,#11079));
#2854=EDGE_LOOP('',(#11080,#11081,#11082,#11083));
#2855=EDGE_LOOP('',(#11084,#11085,#11086,#11087));
#2856=EDGE_LOOP('',(#11088,#11089,#11090,#11091));
#2857=EDGE_LOOP('',(#11092,#11093,#11094,#11095));
#2858=EDGE_LOOP('',(#11096,#11097,#11098,#11099));
#2859=EDGE_LOOP('',(#11100,#11101,#11102,#11103));
#2860=EDGE_LOOP('',(#11104,#11105,#11106,#11107));
#2861=EDGE_LOOP('',(#11108,#11109,#11110,#11111));
#2862=EDGE_LOOP('',(#11112,#11113,#11114,#11115));
#2863=EDGE_LOOP('',(#11116,#11117,#11118,#11119));
#2864=EDGE_LOOP('',(#11120,#11121,#11122,#11123));
#2865=EDGE_LOOP('',(#11124,#11125,#11126,#11127));
#2866=EDGE_LOOP('',(#11128,#11129,#11130,#11131));
#2867=EDGE_LOOP('',(#11132,#11133,#11134,#11135));
#2868=EDGE_LOOP('',(#11136,#11137,#11138,#11139));
#2869=EDGE_LOOP('',(#11140,#11141,#11142,#11143));
#2870=EDGE_LOOP('',(#11144,#11145,#11146,#11147));
#2871=EDGE_LOOP('',(#11148,#11149,#11150,#11151));
#2872=EDGE_LOOP('',(#11152,#11153,#11154,#11155));
#2873=EDGE_LOOP('',(#11156,#11157,#11158,#11159));
#2874=EDGE_LOOP('',(#11160,#11161,#11162,#11163));
#2875=EDGE_LOOP('',(#11164,#11165,#11166,#11167));
#2876=EDGE_LOOP('',(#11168,#11169,#11170,#11171));
#2877=EDGE_LOOP('',(#11172,#11173,#11174,#11175));
#2878=EDGE_LOOP('',(#11176,#11177,#11178,#11179));
#2879=EDGE_LOOP('',(#11180,#11181,#11182,#11183));
#2880=EDGE_LOOP('',(#11184,#11185,#11186,#11187));
#2881=EDGE_LOOP('',(#11188,#11189,#11190,#11191));
#2882=EDGE_LOOP('',(#11192,#11193,#11194,#11195));
#2883=EDGE_LOOP('',(#11196,#11197,#11198,#11199));
#2884=EDGE_LOOP('',(#11200,#11201,#11202,#11203));
#2885=EDGE_LOOP('',(#11204,#11205,#11206,#11207));
#2886=EDGE_LOOP('',(#11208,#11209,#11210,#11211));
#2887=EDGE_LOOP('',(#11212,#11213,#11214,#11215));
#2888=EDGE_LOOP('',(#11216,#11217,#11218,#11219));
#2889=EDGE_LOOP('',(#11220,#11221,#11222,#11223));
#2890=EDGE_LOOP('',(#11224,#11225,#11226,#11227));
#2891=EDGE_LOOP('',(#11228,#11229,#11230,#11231));
#2892=EDGE_LOOP('',(#11232,#11233,#11234,#11235));
#2893=EDGE_LOOP('',(#11236,#11237,#11238,#11239));
#2894=EDGE_LOOP('',(#11240,#11241,#11242,#11243));
#2895=EDGE_LOOP('',(#11244,#11245,#11246,#11247));
#2896=EDGE_LOOP('',(#11248,#11249,#11250,#11251));
#2897=EDGE_LOOP('',(#11252,#11253,#11254,#11255));
#2898=EDGE_LOOP('',(#11256,#11257,#11258,#11259));
#2899=EDGE_LOOP('',(#11260,#11261,#11262,#11263));
#2900=EDGE_LOOP('',(#11264,#11265,#11266,#11267));
#2901=EDGE_LOOP('',(#11268,#11269,#11270,#11271));
#2902=EDGE_LOOP('',(#11272,#11273,#11274,#11275));
#2903=EDGE_LOOP('',(#11276,#11277,#11278,#11279));
#2904=EDGE_LOOP('',(#11280,#11281,#11282,#11283));
#2905=EDGE_LOOP('',(#11284,#11285,#11286,#11287));
#2906=EDGE_LOOP('',(#11288,#11289,#11290,#11291));
#2907=EDGE_LOOP('',(#11292,#11293,#11294,#11295));
#2908=EDGE_LOOP('',(#11296,#11297,#11298,#11299));
#2909=EDGE_LOOP('',(#11300,#11301,#11302,#11303));
#2910=EDGE_LOOP('',(#11304,#11305,#11306,#11307));
#2911=EDGE_LOOP('',(#11308,#11309,#11310,#11311));
#2912=EDGE_LOOP('',(#11312,#11313,#11314,#11315));
#2913=EDGE_LOOP('',(#11316,#11317,#11318,#11319));
#2914=EDGE_LOOP('',(#11320,#11321,#11322,#11323));
#2915=EDGE_LOOP('',(#11324,#11325,#11326,#11327));
#2916=EDGE_LOOP('',(#11328,#11329,#11330,#11331));
#2917=EDGE_LOOP('',(#11332,#11333,#11334,#11335));
#2918=EDGE_LOOP('',(#11336,#11337,#11338,#11339));
#2919=EDGE_LOOP('',(#11340,#11341,#11342,#11343));
#2920=EDGE_LOOP('',(#11344,#11345,#11346,#11347));
#2921=EDGE_LOOP('',(#11348,#11349,#11350,#11351));
#2922=EDGE_LOOP('',(#11352,#11353,#11354,#11355));
#2923=EDGE_LOOP('',(#11356,#11357,#11358,#11359,#11360,#11361,#11362,#11363,
#11364,#11365,#11366,#11367,#11368,#11369,#11370,#11371,#11372,#11373,#11374,
#11375,#11376,#11377,#11378,#11379,#11380,#11381,#11382,#11383,#11384,#11385,
#11386,#11387,#11388,#11389,#11390,#11391,#11392,#11393,#11394,#11395,#11396,
#11397,#11398,#11399,#11400,#11401,#11402,#11403,#11404,#11405,#11406,#11407,
#11408,#11409,#11410,#11411,#11412,#11413,#11414,#11415,#11416,#11417,#11418,
#11419,#11420,#11421,#11422,#11423,#11424,#11425,#11426,#11427,#11428,#11429,
#11430,#11431,#11432,#11433,#11434,#11435,#11436,#11437,#11438,#11439,#11440,
#11441,#11442,#11443,#11444,#11445,#11446,#11447,#11448,#11449,#11450,#11451,
#11452,#11453,#11454,#11455,#11456,#11457,#11458,#11459,#11460,#11461,#11462,
#11463,#11464,#11465,#11466,#11467,#11468,#11469,#11470,#11471,#11472,#11473,
#11474,#11475,#11476,#11477,#11478,#11479,#11480,#11481,#11482,#11483));
#2924=EDGE_LOOP('',(#11484,#11485,#11486,#11487,#11488,#11489,#11490,#11491,
#11492,#11493,#11494,#11495,#11496,#11497,#11498,#11499,#11500,#11501,#11502,
#11503,#11504,#11505,#11506,#11507,#11508,#11509,#11510,#11511,#11512,#11513,
#11514,#11515,#11516,#11517,#11518,#11519,#11520,#11521,#11522,#11523,#11524,
#11525,#11526,#11527,#11528,#11529,#11530,#11531,#11532,#11533,#11534,#11535,
#11536,#11537,#11538,#11539,#11540,#11541,#11542,#11543,#11544,#11545,#11546,
#11547,#11548,#11549,#11550,#11551,#11552,#11553,#11554,#11555,#11556,#11557,
#11558,#11559,#11560,#11561,#11562,#11563,#11564,#11565,#11566,#11567,#11568,
#11569,#11570,#11571,#11572,#11573,#11574,#11575,#11576,#11577,#11578,#11579,
#11580,#11581,#11582,#11583,#11584,#11585,#11586,#11587,#11588,#11589,#11590,
#11591,#11592,#11593,#11594,#11595,#11596,#11597,#11598,#11599,#11600,#11601,
#11602,#11603,#11604,#11605,#11606,#11607,#11608,#11609,#11610,#11611));
#2925=EDGE_LOOP('',(#11612,#11613));
#2926=EDGE_LOOP('',(#11614,#11615,#11616,#11617,#11618,#11619,#11620,#11621));
#2927=EDGE_LOOP('',(#11622,#11623));
#2928=EDGE_LOOP('',(#11624,#11625,#11626,#11627,#11628,#11629,#11630,#11631));
#2929=EDGE_LOOP('',(#11632,#11633));
#2930=EDGE_LOOP('',(#11634,#11635,#11636,#11637,#11638,#11639,#11640,#11641));
#2931=EDGE_LOOP('',(#11642,#11643));
#2932=EDGE_LOOP('',(#11644,#11645,#11646,#11647,#11648,#11649,#11650,#11651));
#2933=EDGE_LOOP('',(#11652,#11653,#11654,#11655,#11656,#11657,#11658,#11659,
#11660,#11661,#11662,#11663));
#2934=EDGE_LOOP('',(#11664,#11665,#11666,#11667,#11668,#11669,#11670,#11671,
#11672,#11673,#11674,#11675));
#2935=EDGE_LOOP('',(#11676,#11677,#11678,#11679,#11680,#11681,#11682,#11683,
#11684,#11685,#11686,#11687));
#2936=EDGE_LOOP('',(#11688,#11689,#11690,#11691,#11692,#11693,#11694,#11695,
#11696,#11697));
#2937=EDGE_LOOP('',(#11698,#11699,#11700,#11701));
#2938=EDGE_LOOP('',(#11702,#11703,#11704,#11705));
#2939=EDGE_LOOP('',(#11706));
#2940=EDGE_LOOP('',(#11707));
#2941=EDGE_LOOP('',(#11708));
#2942=EDGE_LOOP('',(#11709));
#2943=EDGE_LOOP('',(#11710,#11711,#11712,#11713));
#2944=EDGE_LOOP('',(#11714,#11715,#11716,#11717,#11718,#11719,#11720,#11721,
#11722,#11723));
#2945=EDGE_LOOP('',(#11724,#11725,#11726,#11727));
#2946=EDGE_LOOP('',(#11728,#11729,#11730,#11731));
#2947=EDGE_LOOP('',(#11732,#11733,#11734,#11735));
#2948=EDGE_LOOP('',(#11736,#11737,#11738,#11739));
#2949=EDGE_LOOP('',(#11740,#11741,#11742,#11743));
#2950=EDGE_LOOP('',(#11744,#11745,#11746,#11747,#11748,#11749,#11750,#11751,
#11752,#11753,#11754,#11755));
#2951=EDGE_LOOP('',(#11756,#11757,#11758,#11759));
#2952=EDGE_LOOP('',(#11760,#11761,#11762,#11763));
#2953=EDGE_LOOP('',(#11764,#11765,#11766,#11767));
#2954=EDGE_LOOP('',(#11768,#11769,#11770,#11771));
#2955=EDGE_LOOP('',(#11772,#11773,#11774,#11775));
#2956=EDGE_LOOP('',(#11776,#11777,#11778,#11779));
#2957=EDGE_LOOP('',(#11780,#11781,#11782,#11783));
#2958=EDGE_LOOP('',(#11784,#11785,#11786,#11787));
#2959=EDGE_LOOP('',(#11788,#11789,#11790,#11791,#11792,#11793,#11794,#11795));
#2960=EDGE_LOOP('',(#11796,#11797,#11798,#11799,#11800,#11801,#11802,#11803));
#2961=EDGE_LOOP('',(#11804,#11805,#11806,#11807));
#2962=EDGE_LOOP('',(#11808,#11809,#11810,#11811));
#2963=EDGE_LOOP('',(#11812,#11813,#11814,#11815));
#2964=EDGE_LOOP('',(#11816,#11817,#11818,#11819));
#2965=EDGE_LOOP('',(#11820,#11821,#11822,#11823));
#2966=EDGE_LOOP('',(#11824,#11825,#11826,#11827));
#2967=EDGE_LOOP('',(#11828,#11829,#11830,#11831));
#2968=EDGE_LOOP('',(#11832,#11833,#11834,#11835));
#2969=EDGE_LOOP('',(#11836,#11837,#11838,#11839,#11840,#11841,#11842,#11843));
#2970=EDGE_LOOP('',(#11844,#11845,#11846,#11847,#11848,#11849,#11850,#11851));
#2971=EDGE_LOOP('',(#11852,#11853,#11854,#11855));
#2972=EDGE_LOOP('',(#11856,#11857,#11858,#11859));
#2973=EDGE_LOOP('',(#11860,#11861,#11862,#11863));
#2974=EDGE_LOOP('',(#11864,#11865,#11866,#11867));
#2975=EDGE_LOOP('',(#11868,#11869,#11870,#11871));
#2976=EDGE_LOOP('',(#11872,#11873,#11874,#11875));
#2977=EDGE_LOOP('',(#11876,#11877,#11878,#11879,#11880,#11881));
#2978=EDGE_LOOP('',(#11882,#11883,#11884,#11885,#11886,#11887));
#2979=EDGE_LOOP('',(#11888));
#2980=EDGE_LOOP('',(#11889));
#2981=EDGE_LOOP('',(#11890,#11891,#11892,#11893));
#2982=EDGE_LOOP('',(#11894,#11895,#11896,#11897));
#2983=EDGE_LOOP('',(#11898,#11899,#11900,#11901));
#2984=EDGE_LOOP('',(#11902));
#2985=EDGE_LOOP('',(#11903));
#2986=EDGE_LOOP('',(#11904,#11905,#11906,#11907));
#2987=EDGE_LOOP('',(#11908,#11909,#11910,#11911));
#2988=EDGE_LOOP('',(#11912,#11913,#11914,#11915));
#2989=EDGE_LOOP('',(#11916,#11917,#11918,#11919));
#2990=EDGE_LOOP('',(#11920,#11921,#11922,#11923));
#2991=EDGE_LOOP('',(#11924,#11925,#11926,#11927));
#2992=EDGE_LOOP('',(#11928,#11929,#11930,#11931));
#2993=EDGE_LOOP('',(#11932,#11933,#11934,#11935));
#2994=EDGE_LOOP('',(#11936));
#2995=EDGE_LOOP('',(#11937,#11938,#11939,#11940));
#2996=EDGE_LOOP('',(#11941));
#2997=EDGE_LOOP('',(#11942,#11943,#11944,#11945));
#2998=EDGE_LOOP('',(#11946,#11947,#11948,#11949));
#2999=EDGE_LOOP('',(#11950,#11951,#11952,#11953));
#3000=EDGE_LOOP('',(#11954,#11955,#11956,#11957));
#3001=EDGE_LOOP('',(#11958,#11959,#11960,#11961));
#3002=EDGE_LOOP('',(#11962));
#3003=EDGE_LOOP('',(#11963));
#3004=EDGE_LOOP('',(#11964));
#3005=EDGE_LOOP('',(#11965));
#3006=EDGE_LOOP('',(#11966,#11967,#11968,#11969));
#3007=EDGE_LOOP('',(#11970,#11971,#11972,#11973));
#3008=EDGE_LOOP('',(#11974,#11975,#11976,#11977));
#3009=EDGE_LOOP('',(#11978,#11979,#11980,#11981));
#3010=EDGE_LOOP('',(#11982,#11983,#11984,#11985));
#3011=EDGE_LOOP('',(#11986));
#3012=EDGE_LOOP('',(#11987));
#3013=EDGE_LOOP('',(#11988));
#3014=EDGE_LOOP('',(#11989));
#3015=EDGE_LOOP('',(#11990,#11991,#11992,#11993));
#3016=EDGE_LOOP('',(#11994,#11995,#11996,#11997));
#3017=EDGE_LOOP('',(#11998));
#3018=EDGE_LOOP('',(#11999));
#3019=EDGE_LOOP('',(#12000));
#3020=EDGE_LOOP('',(#12001));
#3021=EDGE_LOOP('',(#12002,#12003,#12004,#12005));
#3022=EDGE_LOOP('',(#12006,#12007,#12008,#12009));
#3023=EDGE_LOOP('',(#12010));
#3024=EDGE_LOOP('',(#12011));
#3025=EDGE_LOOP('',(#12012));
#3026=EDGE_LOOP('',(#12013));
#3027=EDGE_LOOP('',(#12014,#12015,#12016,#12017));
#3028=EDGE_LOOP('',(#12018,#12019,#12020,#12021));
#3029=EDGE_LOOP('',(#12022));
#3030=EDGE_LOOP('',(#12023));
#3031=EDGE_LOOP('',(#12024));
#3032=EDGE_LOOP('',(#12025));
#3033=EDGE_LOOP('',(#12026,#12027,#12028,#12029));
#3034=EDGE_LOOP('',(#12030,#12031,#12032,#12033));
#3035=EDGE_LOOP('',(#12034));
#3036=EDGE_LOOP('',(#12035));
#3037=EDGE_LOOP('',(#12036));
#3038=EDGE_LOOP('',(#12037));
#3039=EDGE_LOOP('',(#12038,#12039,#12040,#12041));
#3040=EDGE_LOOP('',(#12042,#12043,#12044,#12045));
#3041=EDGE_LOOP('',(#12046));
#3042=EDGE_LOOP('',(#12047));
#3043=EDGE_LOOP('',(#12048));
#3044=EDGE_LOOP('',(#12049));
#3045=EDGE_LOOP('',(#12050,#12051,#12052,#12053));
#3046=EDGE_LOOP('',(#12054,#12055,#12056,#12057));
#3047=EDGE_LOOP('',(#12058));
#3048=EDGE_LOOP('',(#12059));
#3049=EDGE_LOOP('',(#12060));
#3050=EDGE_LOOP('',(#12061));
#3051=EDGE_LOOP('',(#12062,#12063,#12064,#12065));
#3052=EDGE_LOOP('',(#12066,#12067,#12068,#12069));
#3053=EDGE_LOOP('',(#12070,#12071,#12072,#12073));
#3054=EDGE_LOOP('',(#12074,#12075,#12076,#12077));
#3055=EDGE_LOOP('',(#12078));
#3056=EDGE_LOOP('',(#12079,#12080,#12081,#12082));
#3057=EDGE_LOOP('',(#12083,#12084,#12085,#12086));
#3058=EDGE_LOOP('',(#12087,#12088,#12089,#12090));
#3059=EDGE_LOOP('',(#12091,#12092,#12093,#12094));
#3060=EDGE_LOOP('',(#12095,#12096,#12097,#12098));
#3061=EDGE_LOOP('',(#12099));
#3062=EDGE_LOOP('',(#12100,#12101,#12102,#12103));
#3063=EDGE_LOOP('',(#12104,#12105,#12106,#12107));
#3064=EDGE_LOOP('',(#12108));
#3065=EDGE_LOOP('',(#12109,#12110,#12111,#12112));
#3066=EDGE_LOOP('',(#12113,#12114,#12115,#12116));
#3067=EDGE_LOOP('',(#12117));
#3068=EDGE_LOOP('',(#12118,#12119,#12120,#12121));
#3069=EDGE_LOOP('',(#12122,#12123,#12124,#12125));
#3070=EDGE_LOOP('',(#12126,#12127,#12128,#12129));
#3071=EDGE_LOOP('',(#12130));
#3072=EDGE_LOOP('',(#12131));
#3073=EDGE_LOOP('',(#12132));
#3074=EDGE_LOOP('',(#12133));
#3075=EDGE_LOOP('',(#12134,#12135,#12136,#12137));
#3076=EDGE_LOOP('',(#12138,#12139,#12140,#12141));
#3077=EDGE_LOOP('',(#12142,#12143,#12144,#12145));
#3078=EDGE_LOOP('',(#12146,#12147,#12148,#12149,#12150,#12151,#12152,#12153,
#12154,#12155,#12156,#12157,#12158,#12159,#12160,#12161,#12162,#12163,#12164,
#12165,#12166,#12167,#12168,#12169,#12170,#12171,#12172,#12173,#12174,#12175,
#12176,#12177,#12178,#12179,#12180,#12181,#12182,#12183,#12184,#12185,#12186,
#12187,#12188,#12189,#12190,#12191,#12192,#12193,#12194,#12195,#12196,#12197,
#12198,#12199,#12200,#12201,#12202,#12203,#12204,#12205,#12206,#12207,#12208,
#12209,#12210,#12211,#12212,#12213,#12214,#12215,#12216,#12217,#12218,#12219,
#12220,#12221,#12222,#12223,#12224,#12225));
#3079=EDGE_LOOP('',(#12226,#12227,#12228,#12229));
#3080=EDGE_LOOP('',(#12230,#12231,#12232,#12233));
#3081=EDGE_LOOP('',(#12234,#12235,#12236,#12237));
#3082=EDGE_LOOP('',(#12238));
#3083=EDGE_LOOP('',(#12239,#12240,#12241,#12242));
#3084=EDGE_LOOP('',(#12243,#12244,#12245,#12246));
#3085=EDGE_LOOP('',(#12247,#12248,#12249,#12250));
#3086=EDGE_LOOP('',(#12251,#12252,#12253,#12254));
#3087=EDGE_LOOP('',(#12255,#12256,#12257,#12258));
#3088=EDGE_LOOP('',(#12259,#12260,#12261,#12262));
#3089=EDGE_LOOP('',(#12263,#12264,#12265,#12266));
#3090=EDGE_LOOP('',(#12267,#12268,#12269,#12270));
#3091=EDGE_LOOP('',(#12271,#12272,#12273,#12274));
#3092=EDGE_LOOP('',(#12275,#12276,#12277,#12278));
#3093=EDGE_LOOP('',(#12279,#12280,#12281,#12282));
#3094=EDGE_LOOP('',(#12283,#12284,#12285,#12286));
#3095=EDGE_LOOP('',(#12287,#12288,#12289,#12290));
#3096=EDGE_LOOP('',(#12291,#12292,#12293,#12294));
#3097=EDGE_LOOP('',(#12295,#12296,#12297,#12298));
#3098=EDGE_LOOP('',(#12299,#12300,#12301,#12302));
#3099=EDGE_LOOP('',(#12303,#12304,#12305,#12306));
#3100=EDGE_LOOP('',(#12307,#12308,#12309,#12310));
#3101=EDGE_LOOP('',(#12311,#12312,#12313,#12314));
#3102=EDGE_LOOP('',(#12315,#12316,#12317,#12318));
#3103=EDGE_LOOP('',(#12319,#12320,#12321,#12322));
#3104=EDGE_LOOP('',(#12323,#12324,#12325,#12326));
#3105=EDGE_LOOP('',(#12327,#12328,#12329,#12330));
#3106=EDGE_LOOP('',(#12331,#12332,#12333,#12334));
#3107=EDGE_LOOP('',(#12335,#12336,#12337,#12338));
#3108=EDGE_LOOP('',(#12339,#12340,#12341,#12342));
#3109=EDGE_LOOP('',(#12343,#12344,#12345,#12346));
#3110=EDGE_LOOP('',(#12347,#12348,#12349,#12350));
#3111=EDGE_LOOP('',(#12351,#12352,#12353,#12354));
#3112=EDGE_LOOP('',(#12355,#12356,#12357,#12358));
#3113=EDGE_LOOP('',(#12359,#12360,#12361,#12362));
#3114=EDGE_LOOP('',(#12363,#12364,#12365,#12366));
#3115=EDGE_LOOP('',(#12367,#12368,#12369,#12370));
#3116=EDGE_LOOP('',(#12371,#12372,#12373,#12374));
#3117=EDGE_LOOP('',(#12375,#12376,#12377,#12378));
#3118=EDGE_LOOP('',(#12379,#12380,#12381,#12382));
#3119=EDGE_LOOP('',(#12383,#12384,#12385,#12386));
#3120=EDGE_LOOP('',(#12387,#12388,#12389,#12390));
#3121=EDGE_LOOP('',(#12391,#12392,#12393,#12394));
#3122=EDGE_LOOP('',(#12395,#12396,#12397,#12398));
#3123=EDGE_LOOP('',(#12399,#12400,#12401,#12402));
#3124=EDGE_LOOP('',(#12403,#12404,#12405,#12406));
#3125=EDGE_LOOP('',(#12407,#12408,#12409,#12410));
#3126=EDGE_LOOP('',(#12411,#12412,#12413,#12414));
#3127=EDGE_LOOP('',(#12415,#12416,#12417,#12418));
#3128=EDGE_LOOP('',(#12419,#12420,#12421,#12422));
#3129=EDGE_LOOP('',(#12423,#12424,#12425,#12426));
#3130=EDGE_LOOP('',(#12427,#12428,#12429,#12430));
#3131=EDGE_LOOP('',(#12431,#12432,#12433,#12434));
#3132=EDGE_LOOP('',(#12435,#12436,#12437,#12438));
#3133=EDGE_LOOP('',(#12439,#12440,#12441,#12442));
#3134=EDGE_LOOP('',(#12443,#12444,#12445,#12446));
#3135=EDGE_LOOP('',(#12447,#12448,#12449,#12450));
#3136=EDGE_LOOP('',(#12451,#12452,#12453,#12454));
#3137=EDGE_LOOP('',(#12455,#12456,#12457,#12458));
#3138=EDGE_LOOP('',(#12459,#12460,#12461,#12462));
#3139=EDGE_LOOP('',(#12463,#12464,#12465,#12466));
#3140=EDGE_LOOP('',(#12467,#12468,#12469,#12470));
#3141=EDGE_LOOP('',(#12471,#12472,#12473,#12474));
#3142=EDGE_LOOP('',(#12475,#12476,#12477,#12478));
#3143=EDGE_LOOP('',(#12479,#12480,#12481,#12482));
#3144=EDGE_LOOP('',(#12483,#12484,#12485,#12486));
#3145=EDGE_LOOP('',(#12487,#12488,#12489,#12490));
#3146=EDGE_LOOP('',(#12491,#12492,#12493,#12494));
#3147=EDGE_LOOP('',(#12495,#12496,#12497,#12498));
#3148=EDGE_LOOP('',(#12499,#12500,#12501,#12502));
#3149=EDGE_LOOP('',(#12503,#12504,#12505,#12506));
#3150=EDGE_LOOP('',(#12507,#12508,#12509,#12510));
#3151=EDGE_LOOP('',(#12511,#12512,#12513,#12514));
#3152=EDGE_LOOP('',(#12515,#12516,#12517,#12518));
#3153=EDGE_LOOP('',(#12519,#12520,#12521,#12522));
#3154=EDGE_LOOP('',(#12523,#12524,#12525,#12526));
#3155=EDGE_LOOP('',(#12527,#12528,#12529,#12530));
#3156=EDGE_LOOP('',(#12531,#12532,#12533,#12534));
#3157=EDGE_LOOP('',(#12535,#12536,#12537,#12538));
#3158=EDGE_LOOP('',(#12539,#12540,#12541,#12542));
#3159=EDGE_LOOP('',(#12543,#12544,#12545,#12546));
#3160=EDGE_LOOP('',(#12547,#12548,#12549,#12550));
#3161=EDGE_LOOP('',(#12551,#12552,#12553,#12554));
#3162=EDGE_LOOP('',(#12555,#12556,#12557,#12558));
#3163=EDGE_LOOP('',(#12559,#12560,#12561,#12562,#12563,#12564,#12565,#12566,
#12567,#12568,#12569,#12570,#12571,#12572,#12573,#12574,#12575,#12576,#12577,
#12578,#12579,#12580,#12581,#12582,#12583,#12584,#12585,#12586,#12587,#12588,
#12589,#12590,#12591,#12592,#12593,#12594,#12595,#12596,#12597,#12598,#12599,
#12600,#12601,#12602,#12603,#12604,#12605,#12606,#12607,#12608,#12609,#12610,
#12611,#12612,#12613,#12614,#12615,#12616,#12617,#12618,#12619,#12620,#12621,
#12622,#12623,#12624,#12625,#12626,#12627,#12628,#12629,#12630,#12631,#12632,
#12633,#12634,#12635,#12636,#12637,#12638));
#3164=EDGE_LOOP('',(#12639));
#3165=EDGE_LOOP('',(#12640,#12641,#12642,#12643));
#3166=EDGE_LOOP('',(#12644));
#3167=EDGE_LOOP('',(#12645,#12646,#12647,#12648));
#3168=EDGE_LOOP('',(#12649,#12650,#12651,#12652));
#3169=EDGE_LOOP('',(#12653,#12654,#12655,#12656));
#3170=EDGE_LOOP('',(#12657));
#3171=EDGE_LOOP('',(#12658));
#3172=EDGE_LOOP('',(#12659,#12660,#12661,#12662));
#3173=EDGE_LOOP('',(#12663,#12664,#12665,#12666));
#3174=EDGE_LOOP('',(#12667,#12668,#12669,#12670));
#3175=EDGE_LOOP('',(#12671));
#3176=EDGE_LOOP('',(#12672,#12673,#12674,#12675));
#3177=EDGE_LOOP('',(#12676,#12677,#12678,#12679));
#3178=EDGE_LOOP('',(#12680,#12681,#12682,#12683));
#3179=EDGE_LOOP('',(#12684,#12685,#12686,#12687));
#3180=EDGE_LOOP('',(#12688,#12689,#12690,#12691));
#3181=EDGE_LOOP('',(#12692,#12693,#12694,#12695));
#3182=EDGE_LOOP('',(#12696,#12697,#12698,#12699,#12700,#12701));
#3183=EDGE_LOOP('',(#12702,#12703,#12704,#12705,#12706,#12707));
#3184=EDGE_LOOP('',(#12708,#12709,#12710,#12711,#12712,#12713,#12714,#12715));
#3185=EDGE_LOOP('',(#12716,#12717,#12718,#12719));
#3186=EDGE_LOOP('',(#12720,#12721,#12722,#12723));
#3187=EDGE_LOOP('',(#12724,#12725,#12726,#12727));
#3188=EDGE_LOOP('',(#12728,#12729,#12730,#12731));
#3189=EDGE_LOOP('',(#12732,#12733,#12734,#12735,#12736,#12737,#12738,#12739));
#3190=EDGE_LOOP('',(#12740,#12741,#12742,#12743));
#3191=EDGE_LOOP('',(#12744,#12745,#12746,#12747));
#3192=EDGE_LOOP('',(#12748,#12749,#12750,#12751));
#3193=EDGE_LOOP('',(#12752,#12753,#12754,#12755));
#3194=EDGE_LOOP('',(#12756,#12757,#12758,#12759));
#3195=EDGE_LOOP('',(#12760,#12761,#12762,#12763));
#3196=EDGE_LOOP('',(#12764));
#3197=EDGE_LOOP('',(#12765));
#3198=EDGE_LOOP('',(#12766));
#3199=EDGE_LOOP('',(#12767));
#3200=EDGE_LOOP('',(#12768));
#3201=EDGE_LOOP('',(#12769,#12770,#12771,#12772));
#3202=EDGE_LOOP('',(#12773,#12774,#12775,#12776));
#3203=EDGE_LOOP('',(#12777,#12778,#12779,#12780));
#3204=EDGE_LOOP('',(#12781));
#3205=EDGE_LOOP('',(#12782));
#3206=EDGE_LOOP('',(#12783,#12784,#12785,#12786));
#3207=EDGE_LOOP('',(#12787,#12788,#12789,#12790));
#3208=EDGE_LOOP('',(#12791,#12792,#12793,#12794));
#3209=EDGE_LOOP('',(#12795));
#3210=EDGE_LOOP('',(#12796,#12797,#12798,#12799));
#3211=EDGE_LOOP('',(#12800,#12801,#12802,#12803));
#3212=EDGE_LOOP('',(#12804,#12805,#12806,#12807));
#3213=EDGE_LOOP('',(#12808,#12809,#12810,#12811));
#3214=EDGE_LOOP('',(#12812,#12813,#12814,#12815));
#3215=EDGE_LOOP('',(#12816,#12817,#12818,#12819));
#3216=EDGE_LOOP('',(#12820,#12821,#12822,#12823,#12824,#12825));
#3217=EDGE_LOOP('',(#12826,#12827,#12828,#12829,#12830,#12831));
#3218=EDGE_LOOP('',(#12832,#12833,#12834,#12835));
#3219=EDGE_LOOP('',(#12836,#12837,#12838,#12839));
#3220=EDGE_LOOP('',(#12840));
#3221=EDGE_LOOP('',(#12841));
#3222=EDGE_LOOP('',(#12842));
#3223=EDGE_LOOP('',(#12843));
#3224=LINE('',#19464,#4515);
#3225=LINE('',#19470,#4516);
#3226=LINE('',#19476,#4517);
#3227=LINE('',#19482,#4518);
#3228=LINE('',#19487,#4519);
#3229=LINE('',#19489,#4520);
#3230=LINE('',#19491,#4521);
#3231=LINE('',#19492,#4522);
#3232=LINE('',#19495,#4523);
#3233=LINE('',#19497,#4524);
#3234=LINE('',#19498,#4525);
#3235=LINE('',#19501,#4526);
#3236=LINE('',#19503,#4527);
#3237=LINE('',#19504,#4528);
#3238=LINE('',#19506,#4529);
#3239=LINE('',#19507,#4530);
#3240=LINE('',#19514,#4531);
#3241=LINE('',#19516,#4532);
#3242=LINE('',#19518,#4533);
#3243=LINE('',#19519,#4534);
#3244=LINE('',#19522,#4535);
#3245=LINE('',#19524,#4536);
#3246=LINE('',#19525,#4537);
#3247=LINE('',#19528,#4538);
#3248=LINE('',#19530,#4539);
#3249=LINE('',#19531,#4540);
#3250=LINE('',#19533,#4541);
#3251=LINE('',#19534,#4542);
#3252=LINE('',#19541,#4543);
#3253=LINE('',#19543,#4544);
#3254=LINE('',#19545,#4545);
#3255=LINE('',#19546,#4546);
#3256=LINE('',#19549,#4547);
#3257=LINE('',#19551,#4548);
#3258=LINE('',#19552,#4549);
#3259=LINE('',#19555,#4550);
#3260=LINE('',#19557,#4551);
#3261=LINE('',#19558,#4552);
#3262=LINE('',#19560,#4553);
#3263=LINE('',#19561,#4554);
#3264=LINE('',#19569,#4555);
#3265=LINE('',#19575,#4556);
#3266=LINE('',#19581,#4557);
#3267=LINE('',#19587,#4558);
#3268=LINE('',#19593,#4559);
#3269=LINE('',#19599,#4560);
#3270=LINE('',#19605,#4561);
#3271=LINE('',#19611,#4562);
#3272=LINE('',#19617,#4563);
#3273=LINE('',#19623,#4564);
#3274=LINE('',#19629,#4565);
#3275=LINE('',#19635,#4566);
#3276=LINE('',#19641,#4567);
#3277=LINE('',#19647,#4568);
#3278=LINE('',#19653,#4569);
#3279=LINE('',#19659,#4570);
#3280=LINE('',#19664,#4571);
#3281=LINE('',#19666,#4572);
#3282=LINE('',#19668,#4573);
#3283=LINE('',#19669,#4574);
#3284=LINE('',#19672,#4575);
#3285=LINE('',#19674,#4576);
#3286=LINE('',#19675,#4577);
#3287=LINE('',#19678,#4578);
#3288=LINE('',#19680,#4579);
#3289=LINE('',#19681,#4580);
#3290=LINE('',#19683,#4581);
#3291=LINE('',#19684,#4582);
#3292=LINE('',#19692,#4583);
#3293=LINE('',#19701,#4584);
#3294=LINE('',#19709,#4585);
#3295=LINE('',#19713,#4586);
#3296=LINE('',#19717,#4587);
#3297=LINE('',#19719,#4588);
#3298=LINE('',#19721,#4589);
#3299=LINE('',#19722,#4590);
#3300=LINE('',#19725,#4591);
#3301=LINE('',#19727,#4592);
#3302=LINE('',#19728,#4593);
#3303=LINE('',#19731,#4594);
#3304=LINE('',#19733,#4595);
#3305=LINE('',#19734,#4596);
#3306=LINE('',#19736,#4597);
#3307=LINE('',#19737,#4598);
#3308=LINE('',#19744,#4599);
#3309=LINE('',#19746,#4600);
#3310=LINE('',#19748,#4601);
#3311=LINE('',#19749,#4602);
#3312=LINE('',#19752,#4603);
#3313=LINE('',#19754,#4604);
#3314=LINE('',#19755,#4605);
#3315=LINE('',#19758,#4606);
#3316=LINE('',#19760,#4607);
#3317=LINE('',#19761,#4608);
#3318=LINE('',#19763,#4609);
#3319=LINE('',#19764,#4610);
#3320=LINE('',#19772,#4611);
#3321=LINE('',#19781,#4612);
#3322=LINE('',#19789,#4613);
#3323=LINE('',#19793,#4614);
#3324=LINE('',#19797,#4615);
#3325=LINE('',#19799,#4616);
#3326=LINE('',#19801,#4617);
#3327=LINE('',#19802,#4618);
#3328=LINE('',#19805,#4619);
#3329=LINE('',#19807,#4620);
#3330=LINE('',#19808,#4621);
#3331=LINE('',#19811,#4622);
#3332=LINE('',#19813,#4623);
#3333=LINE('',#19814,#4624);
#3334=LINE('',#19816,#4625);
#3335=LINE('',#19817,#4626);
#3336=LINE('',#19824,#4627);
#3337=LINE('',#19826,#4628);
#3338=LINE('',#19828,#4629);
#3339=LINE('',#19829,#4630);
#3340=LINE('',#19832,#4631);
#3341=LINE('',#19834,#4632);
#3342=LINE('',#19835,#4633);
#3343=LINE('',#19838,#4634);
#3344=LINE('',#19840,#4635);
#3345=LINE('',#19841,#4636);
#3346=LINE('',#19843,#4637);
#3347=LINE('',#19844,#4638);
#3348=LINE('',#19852,#4639);
#3349=LINE('',#19858,#4640);
#3350=LINE('',#19864,#4641);
#3351=LINE('',#19870,#4642);
#3352=LINE('',#19876,#4643);
#3353=LINE('',#19882,#4644);
#3354=LINE('',#19888,#4645);
#3355=LINE('',#19893,#4646);
#3356=LINE('',#19895,#4647);
#3357=LINE('',#19897,#4648);
#3358=LINE('',#19898,#4649);
#3359=LINE('',#19902,#4650);
#3360=LINE('',#19904,#4651);
#3361=LINE('',#19906,#4652);
#3362=LINE('',#19907,#4653);
#3363=LINE('',#19910,#4654);
#3364=LINE('',#19912,#4655);
#3365=LINE('',#19913,#4656);
#3366=LINE('',#19916,#4657);
#3367=LINE('',#19918,#4658);
#3368=LINE('',#19919,#4659);
#3369=LINE('',#19922,#4660);
#3370=LINE('',#19924,#4661);
#3371=LINE('',#19925,#4662);
#3372=LINE('',#19926,#4663);
#3373=LINE('',#19929,#4664);
#3374=LINE('',#19930,#4665);
#3375=LINE('',#19933,#4666);
#3376=LINE('',#19934,#4667);
#3377=LINE('',#19935,#4668);
#3378=LINE('',#19937,#4669);
#3379=LINE('',#19945,#4670);
#3380=LINE('',#19951,#4671);
#3381=LINE('',#19957,#4672);
#3382=LINE('',#19963,#4673);
#3383=LINE('',#19969,#4674);
#3384=LINE('',#19976,#4675);
#3385=LINE('',#19982,#4676);
#3386=LINE('',#19991,#4677);
#3387=LINE('',#19997,#4678);
#3388=LINE('',#20003,#4679);
#3389=LINE('',#20009,#4680);
#3390=LINE('',#20015,#4681);
#3391=LINE('',#20023,#4682);
#3392=LINE('',#20028,#4683);
#3393=LINE('',#20037,#4684);
#3394=LINE('',#20043,#4685);
#3395=LINE('',#20049,#4686);
#3396=LINE('',#20055,#4687);
#3397=LINE('',#20061,#4688);
#3398=LINE('',#20067,#4689);
#3399=LINE('',#20073,#4690);
#3400=LINE('',#20078,#4691);
#3401=LINE('',#20080,#4692);
#3402=LINE('',#20082,#4693);
#3403=LINE('',#20083,#4694);
#3404=LINE('',#20087,#4695);
#3405=LINE('',#20089,#4696);
#3406=LINE('',#20091,#4697);
#3407=LINE('',#20092,#4698);
#3408=LINE('',#20095,#4699);
#3409=LINE('',#20097,#4700);
#3410=LINE('',#20098,#4701);
#3411=LINE('',#20101,#4702);
#3412=LINE('',#20103,#4703);
#3413=LINE('',#20104,#4704);
#3414=LINE('',#20107,#4705);
#3415=LINE('',#20109,#4706);
#3416=LINE('',#20110,#4707);
#3417=LINE('',#20111,#4708);
#3418=LINE('',#20114,#4709);
#3419=LINE('',#20115,#4710);
#3420=LINE('',#20118,#4711);
#3421=LINE('',#20119,#4712);
#3422=LINE('',#20120,#4713);
#3423=LINE('',#20122,#4714);
#3424=LINE('',#20130,#4715);
#3425=LINE('',#20136,#4716);
#3426=LINE('',#20142,#4717);
#3427=LINE('',#20148,#4718);
#3428=LINE('',#20154,#4719);
#3429=LINE('',#20161,#4720);
#3430=LINE('',#20167,#4721);
#3431=LINE('',#20176,#4722);
#3432=LINE('',#20182,#4723);
#3433=LINE('',#20188,#4724);
#3434=LINE('',#20194,#4725);
#3435=LINE('',#20200,#4726);
#3436=LINE('',#20208,#4727);
#3437=LINE('',#20213,#4728);
#3438=LINE('',#20221,#4729);
#3439=LINE('',#20223,#4730);
#3440=LINE('',#20225,#4731);
#3441=LINE('',#20226,#4732);
#3442=LINE('',#20229,#4733);
#3443=LINE('',#20231,#4734);
#3444=LINE('',#20232,#4735);
#3445=LINE('',#20235,#4736);
#3446=LINE('',#20237,#4737);
#3447=LINE('',#20238,#4738);
#3448=LINE('',#20241,#4739);
#3449=LINE('',#20243,#4740);
#3450=LINE('',#20244,#4741);
#3451=LINE('',#20247,#4742);
#3452=LINE('',#20249,#4743);
#3453=LINE('',#20250,#4744);
#3454=LINE('',#20253,#4745);
#3455=LINE('',#20255,#4746);
#3456=LINE('',#20256,#4747);
#3457=LINE('',#20259,#4748);
#3458=LINE('',#20261,#4749);
#3459=LINE('',#20262,#4750);
#3460=LINE('',#20265,#4751);
#3461=LINE('',#20267,#4752);
#3462=LINE('',#20268,#4753);
#3463=LINE('',#20271,#4754);
#3464=LINE('',#20273,#4755);
#3465=LINE('',#20274,#4756);
#3466=LINE('',#20278,#4757);
#3467=LINE('',#20280,#4758);
#3468=LINE('',#20282,#4759);
#3469=LINE('',#20283,#4760);
#3470=LINE('',#20286,#4761);
#3471=LINE('',#20288,#4762);
#3472=LINE('',#20289,#4763);
#3473=LINE('',#20292,#4764);
#3474=LINE('',#20294,#4765);
#3475=LINE('',#20295,#4766);
#3476=LINE('',#20298,#4767);
#3477=LINE('',#20300,#4768);
#3478=LINE('',#20301,#4769);
#3479=LINE('',#20304,#4770);
#3480=LINE('',#20306,#4771);
#3481=LINE('',#20307,#4772);
#3482=LINE('',#20310,#4773);
#3483=LINE('',#20312,#4774);
#3484=LINE('',#20313,#4775);
#3485=LINE('',#20316,#4776);
#3486=LINE('',#20318,#4777);
#3487=LINE('',#20319,#4778);
#3488=LINE('',#20322,#4779);
#3489=LINE('',#20324,#4780);
#3490=LINE('',#20325,#4781);
#3491=LINE('',#20328,#4782);
#3492=LINE('',#20330,#4783);
#3493=LINE('',#20331,#4784);
#3494=LINE('',#20335,#4785);
#3495=LINE('',#20337,#4786);
#3496=LINE('',#20339,#4787);
#3497=LINE('',#20340,#4788);
#3498=LINE('',#20343,#4789);
#3499=LINE('',#20345,#4790);
#3500=LINE('',#20346,#4791);
#3501=LINE('',#20349,#4792);
#3502=LINE('',#20351,#4793);
#3503=LINE('',#20352,#4794);
#3504=LINE('',#20355,#4795);
#3505=LINE('',#20357,#4796);
#3506=LINE('',#20358,#4797);
#3507=LINE('',#20361,#4798);
#3508=LINE('',#20363,#4799);
#3509=LINE('',#20364,#4800);
#3510=LINE('',#20367,#4801);
#3511=LINE('',#20369,#4802);
#3512=LINE('',#20370,#4803);
#3513=LINE('',#20373,#4804);
#3514=LINE('',#20375,#4805);
#3515=LINE('',#20376,#4806);
#3516=LINE('',#20379,#4807);
#3517=LINE('',#20381,#4808);
#3518=LINE('',#20382,#4809);
#3519=LINE('',#20385,#4810);
#3520=LINE('',#20387,#4811);
#3521=LINE('',#20388,#4812);
#3522=LINE('',#20392,#4813);
#3523=LINE('',#20394,#4814);
#3524=LINE('',#20396,#4815);
#3525=LINE('',#20397,#4816);
#3526=LINE('',#20400,#4817);
#3527=LINE('',#20402,#4818);
#3528=LINE('',#20403,#4819);
#3529=LINE('',#20406,#4820);
#3530=LINE('',#20408,#4821);
#3531=LINE('',#20409,#4822);
#3532=LINE('',#20412,#4823);
#3533=LINE('',#20414,#4824);
#3534=LINE('',#20415,#4825);
#3535=LINE('',#20418,#4826);
#3536=LINE('',#20420,#4827);
#3537=LINE('',#20421,#4828);
#3538=LINE('',#20424,#4829);
#3539=LINE('',#20426,#4830);
#3540=LINE('',#20427,#4831);
#3541=LINE('',#20430,#4832);
#3542=LINE('',#20432,#4833);
#3543=LINE('',#20433,#4834);
#3544=LINE('',#20436,#4835);
#3545=LINE('',#20438,#4836);
#3546=LINE('',#20439,#4837);
#3547=LINE('',#20442,#4838);
#3548=LINE('',#20444,#4839);
#3549=LINE('',#20445,#4840);
#3550=LINE('',#20450,#4841);
#3551=LINE('',#20454,#4842);
#3552=LINE('',#20456,#4843);
#3553=LINE('',#20457,#4844);
#3554=LINE('',#20460,#4845);
#3555=LINE('',#20462,#4846);
#3556=LINE('',#20463,#4847);
#3557=LINE('',#20465,#4848);
#3558=LINE('',#20466,#4849);
#3559=LINE('',#20469,#4850);
#3560=LINE('',#20471,#4851);
#3561=LINE('',#20472,#4852);
#3562=LINE('',#20474,#4853);
#3563=LINE('',#20475,#4854);
#3564=LINE('',#20478,#4855);
#3565=LINE('',#20480,#4856);
#3566=LINE('',#20481,#4857);
#3567=LINE('',#20483,#4858);
#3568=LINE('',#20484,#4859);
#3569=LINE('',#20486,#4860);
#3570=LINE('',#20487,#4861);
#3571=LINE('',#20494,#4862);
#3572=LINE('',#20496,#4863);
#3573=LINE('',#20498,#4864);
#3574=LINE('',#20499,#4865);
#3575=LINE('',#20502,#4866);
#3576=LINE('',#20504,#4867);
#3577=LINE('',#20505,#4868);
#3578=LINE('',#20508,#4869);
#3579=LINE('',#20510,#4870);
#3580=LINE('',#20511,#4871);
#3581=LINE('',#20516,#4872);
#3582=LINE('',#20518,#4873);
#3583=LINE('',#20520,#4874);
#3584=LINE('',#20522,#4875);
#3585=LINE('',#20524,#4876);
#3586=LINE('',#20526,#4877);
#3587=LINE('',#20527,#4878);
#3588=LINE('',#20530,#4879);
#3589=LINE('',#20531,#4880);
#3590=LINE('',#20534,#4881);
#3591=LINE('',#20535,#4882);
#3592=LINE('',#20538,#4883);
#3593=LINE('',#20540,#4884);
#3594=LINE('',#20542,#4885);
#3595=LINE('',#20544,#4886);
#3596=LINE('',#20545,#4887);
#3597=LINE('',#20547,#4888);
#3598=LINE('',#20550,#4889);
#3599=LINE('',#20553,#4890);
#3600=LINE('',#20557,#4891);
#3601=LINE('',#20564,#4892);
#3602=LINE('',#20566,#4893);
#3603=LINE('',#20568,#4894);
#3604=LINE('',#20575,#4895);
#3605=LINE('',#20579,#4896);
#3606=LINE('',#20586,#4897);
#3607=LINE('',#20594,#4898);
#3608=LINE('',#20603,#4899);
#3609=LINE('',#20612,#4900);
#3610=LINE('',#20621,#4901);
#3611=LINE('',#20629,#4902);
#3612=LINE('',#20633,#4903);
#3613=LINE('',#20637,#4904);
#3614=LINE('',#20641,#4905);
#3615=LINE('',#20645,#4906);
#3616=LINE('',#20647,#4907);
#3617=LINE('',#20649,#4908);
#3618=LINE('',#20650,#4909);
#3619=LINE('',#20653,#4910);
#3620=LINE('',#20655,#4911);
#3621=LINE('',#20656,#4912);
#3622=LINE('',#20659,#4913);
#3623=LINE('',#20661,#4914);
#3624=LINE('',#20662,#4915);
#3625=LINE('',#20665,#4916);
#3626=LINE('',#20667,#4917);
#3627=LINE('',#20668,#4918);
#3628=LINE('',#20671,#4919);
#3629=LINE('',#20673,#4920);
#3630=LINE('',#20674,#4921);
#3631=LINE('',#20677,#4922);
#3632=LINE('',#20679,#4923);
#3633=LINE('',#20680,#4924);
#3634=LINE('',#20683,#4925);
#3635=LINE('',#20685,#4926);
#3636=LINE('',#20686,#4927);
#3637=LINE('',#20689,#4928);
#3638=LINE('',#20691,#4929);
#3639=LINE('',#20692,#4930);
#3640=LINE('',#20695,#4931);
#3641=LINE('',#20697,#4932);
#3642=LINE('',#20698,#4933);
#3643=LINE('',#20701,#4934);
#3644=LINE('',#20703,#4935);
#3645=LINE('',#20704,#4936);
#3646=LINE('',#20707,#4937);
#3647=LINE('',#20709,#4938);
#3648=LINE('',#20710,#4939);
#3649=LINE('',#20712,#4940);
#3650=LINE('',#20713,#4941);
#3651=LINE('',#20723,#4942);
#3652=LINE('',#20727,#4943);
#3653=LINE('',#20731,#4944);
#3654=LINE('',#20738,#4945);
#3655=LINE('',#20742,#4946);
#3656=LINE('',#20746,#4947);
#3657=LINE('',#20751,#4948);
#3658=LINE('',#20753,#4949);
#3659=LINE('',#20755,#4950);
#3660=LINE('',#20756,#4951);
#3661=LINE('',#20759,#4952);
#3662=LINE('',#20761,#4953);
#3663=LINE('',#20762,#4954);
#3664=LINE('',#20765,#4955);
#3665=LINE('',#20767,#4956);
#3666=LINE('',#20768,#4957);
#3667=LINE('',#20771,#4958);
#3668=LINE('',#20773,#4959);
#3669=LINE('',#20774,#4960);
#3670=LINE('',#20777,#4961);
#3671=LINE('',#20779,#4962);
#3672=LINE('',#20780,#4963);
#3673=LINE('',#20782,#4964);
#3674=LINE('',#20783,#4965);
#3675=LINE('',#20800,#4966);
#3676=LINE('',#20806,#4967);
#3677=LINE('',#20810,#4968);
#3678=LINE('',#20816,#4969);
#3679=LINE('',#20821,#4970);
#3680=LINE('',#20836,#4971);
#3681=LINE('',#20845,#4972);
#3682=LINE('',#20849,#4973);
#3683=LINE('',#20853,#4974);
#3684=LINE('',#20856,#4975);
#3685=LINE('',#20992,#4976);
#3686=LINE('',#21245,#4977);
#3687=LINE('',#21287,#4978);
#3688=LINE('',#21292,#4979);
#3689=LINE('',#21301,#4980);
#3690=LINE('',#21306,#4981);
#3691=LINE('',#21316,#4982);
#3692=LINE('',#21318,#4983);
#3693=LINE('',#21320,#4984);
#3694=LINE('',#21321,#4985);
#3695=LINE('',#21324,#4986);
#3696=LINE('',#21326,#4987);
#3697=LINE('',#21327,#4988);
#3698=LINE('',#21330,#4989);
#3699=LINE('',#21332,#4990);
#3700=LINE('',#21333,#4991);
#3701=LINE('',#21336,#4992);
#3702=LINE('',#21338,#4993);
#3703=LINE('',#21339,#4994);
#3704=LINE('',#21342,#4995);
#3705=LINE('',#21344,#4996);
#3706=LINE('',#21345,#4997);
#3707=LINE('',#21347,#4998);
#3708=LINE('',#21348,#4999);
#3709=LINE('',#21360,#5000);
#3710=LINE('',#21364,#5001);
#3711=LINE('',#21368,#5002);
#3712=LINE('',#21375,#5003);
#3713=LINE('',#21377,#5004);
#3714=LINE('',#21384,#5005);
#3715=LINE('',#21390,#5006);
#3716=LINE('',#21396,#5007);
#3717=LINE('',#21402,#5008);
#3718=LINE('',#21408,#5009);
#3719=LINE('',#21414,#5010);
#3720=LINE('',#21420,#5011);
#3721=LINE('',#21426,#5012);
#3722=LINE('',#21431,#5013);
#3723=LINE('',#21433,#5014);
#3724=LINE('',#21435,#5015);
#3725=LINE('',#21436,#5016);
#3726=LINE('',#21439,#5017);
#3727=LINE('',#21441,#5018);
#3728=LINE('',#21442,#5019);
#3729=LINE('',#21445,#5020);
#3730=LINE('',#21447,#5021);
#3731=LINE('',#21448,#5022);
#3732=LINE('',#21450,#5023);
#3733=LINE('',#21451,#5024);
#3734=LINE('',#21459,#5025);
#3735=LINE('',#21466,#5026);
#3736=LINE('',#21473,#5027);
#3737=LINE('',#21480,#5028);
#3738=LINE('',#21486,#5029);
#3739=LINE('',#21488,#5030);
#3740=LINE('',#21490,#5031);
#3741=LINE('',#21491,#5032);
#3742=LINE('',#21494,#5033);
#3743=LINE('',#21496,#5034);
#3744=LINE('',#21497,#5035);
#3745=LINE('',#21500,#5036);
#3746=LINE('',#21502,#5037);
#3747=LINE('',#21503,#5038);
#3748=LINE('',#21506,#5039);
#3749=LINE('',#21508,#5040);
#3750=LINE('',#21509,#5041);
#3751=LINE('',#21512,#5042);
#3752=LINE('',#21514,#5043);
#3753=LINE('',#21515,#5044);
#3754=LINE('',#21518,#5045);
#3755=LINE('',#21520,#5046);
#3756=LINE('',#21521,#5047);
#3757=LINE('',#21524,#5048);
#3758=LINE('',#21526,#5049);
#3759=LINE('',#21527,#5050);
#3760=LINE('',#21530,#5051);
#3761=LINE('',#21532,#5052);
#3762=LINE('',#21533,#5053);
#3763=LINE('',#21536,#5054);
#3764=LINE('',#21538,#5055);
#3765=LINE('',#21539,#5056);
#3766=LINE('',#21542,#5057);
#3767=LINE('',#21544,#5058);
#3768=LINE('',#21545,#5059);
#3769=LINE('',#21548,#5060);
#3770=LINE('',#21550,#5061);
#3771=LINE('',#21551,#5062);
#3772=LINE('',#21554,#5063);
#3773=LINE('',#21556,#5064);
#3774=LINE('',#21557,#5065);
#3775=LINE('',#21560,#5066);
#3776=LINE('',#21562,#5067);
#3777=LINE('',#21563,#5068);
#3778=LINE('',#21566,#5069);
#3779=LINE('',#21568,#5070);
#3780=LINE('',#21569,#5071);
#3781=LINE('',#21572,#5072);
#3782=LINE('',#21574,#5073);
#3783=LINE('',#21575,#5074);
#3784=LINE('',#21578,#5075);
#3785=LINE('',#21580,#5076);
#3786=LINE('',#21581,#5077);
#3787=LINE('',#21584,#5078);
#3788=LINE('',#21586,#5079);
#3789=LINE('',#21587,#5080);
#3790=LINE('',#21590,#5081);
#3791=LINE('',#21592,#5082);
#3792=LINE('',#21593,#5083);
#3793=LINE('',#21596,#5084);
#3794=LINE('',#21598,#5085);
#3795=LINE('',#21599,#5086);
#3796=LINE('',#21602,#5087);
#3797=LINE('',#21604,#5088);
#3798=LINE('',#21605,#5089);
#3799=LINE('',#21608,#5090);
#3800=LINE('',#21610,#5091);
#3801=LINE('',#21611,#5092);
#3802=LINE('',#21614,#5093);
#3803=LINE('',#21616,#5094);
#3804=LINE('',#21617,#5095);
#3805=LINE('',#21620,#5096);
#3806=LINE('',#21622,#5097);
#3807=LINE('',#21623,#5098);
#3808=LINE('',#21626,#5099);
#3809=LINE('',#21628,#5100);
#3810=LINE('',#21629,#5101);
#3811=LINE('',#21632,#5102);
#3812=LINE('',#21634,#5103);
#3813=LINE('',#21635,#5104);
#3814=LINE('',#21638,#5105);
#3815=LINE('',#21640,#5106);
#3816=LINE('',#21641,#5107);
#3817=LINE('',#21644,#5108);
#3818=LINE('',#21646,#5109);
#3819=LINE('',#21647,#5110);
#3820=LINE('',#21650,#5111);
#3821=LINE('',#21652,#5112);
#3822=LINE('',#21653,#5113);
#3823=LINE('',#21656,#5114);
#3824=LINE('',#21658,#5115);
#3825=LINE('',#21659,#5116);
#3826=LINE('',#21662,#5117);
#3827=LINE('',#21664,#5118);
#3828=LINE('',#21665,#5119);
#3829=LINE('',#21668,#5120);
#3830=LINE('',#21670,#5121);
#3831=LINE('',#21671,#5122);
#3832=LINE('',#21674,#5123);
#3833=LINE('',#21676,#5124);
#3834=LINE('',#21677,#5125);
#3835=LINE('',#21680,#5126);
#3836=LINE('',#21682,#5127);
#3837=LINE('',#21683,#5128);
#3838=LINE('',#21686,#5129);
#3839=LINE('',#21688,#5130);
#3840=LINE('',#21689,#5131);
#3841=LINE('',#21692,#5132);
#3842=LINE('',#21694,#5133);
#3843=LINE('',#21695,#5134);
#3844=LINE('',#21698,#5135);
#3845=LINE('',#21700,#5136);
#3846=LINE('',#21701,#5137);
#3847=LINE('',#21704,#5138);
#3848=LINE('',#21706,#5139);
#3849=LINE('',#21707,#5140);
#3850=LINE('',#21710,#5141);
#3851=LINE('',#21712,#5142);
#3852=LINE('',#21713,#5143);
#3853=LINE('',#21716,#5144);
#3854=LINE('',#21718,#5145);
#3855=LINE('',#21719,#5146);
#3856=LINE('',#21722,#5147);
#3857=LINE('',#21724,#5148);
#3858=LINE('',#21725,#5149);
#3859=LINE('',#21728,#5150);
#3860=LINE('',#21730,#5151);
#3861=LINE('',#21731,#5152);
#3862=LINE('',#21734,#5153);
#3863=LINE('',#21736,#5154);
#3864=LINE('',#21737,#5155);
#3865=LINE('',#21740,#5156);
#3866=LINE('',#21742,#5157);
#3867=LINE('',#21743,#5158);
#3868=LINE('',#21746,#5159);
#3869=LINE('',#21748,#5160);
#3870=LINE('',#21749,#5161);
#3871=LINE('',#21752,#5162);
#3872=LINE('',#21754,#5163);
#3873=LINE('',#21755,#5164);
#3874=LINE('',#21758,#5165);
#3875=LINE('',#21760,#5166);
#3876=LINE('',#21761,#5167);
#3877=LINE('',#21764,#5168);
#3878=LINE('',#21766,#5169);
#3879=LINE('',#21767,#5170);
#3880=LINE('',#21770,#5171);
#3881=LINE('',#21772,#5172);
#3882=LINE('',#21773,#5173);
#3883=LINE('',#21776,#5174);
#3884=LINE('',#21778,#5175);
#3885=LINE('',#21779,#5176);
#3886=LINE('',#21782,#5177);
#3887=LINE('',#21784,#5178);
#3888=LINE('',#21785,#5179);
#3889=LINE('',#21788,#5180);
#3890=LINE('',#21790,#5181);
#3891=LINE('',#21791,#5182);
#3892=LINE('',#21794,#5183);
#3893=LINE('',#21796,#5184);
#3894=LINE('',#21797,#5185);
#3895=LINE('',#21800,#5186);
#3896=LINE('',#21802,#5187);
#3897=LINE('',#21803,#5188);
#3898=LINE('',#21806,#5189);
#3899=LINE('',#21808,#5190);
#3900=LINE('',#21809,#5191);
#3901=LINE('',#21812,#5192);
#3902=LINE('',#21814,#5193);
#3903=LINE('',#21815,#5194);
#3904=LINE('',#21818,#5195);
#3905=LINE('',#21820,#5196);
#3906=LINE('',#21821,#5197);
#3907=LINE('',#21824,#5198);
#3908=LINE('',#21826,#5199);
#3909=LINE('',#21827,#5200);
#3910=LINE('',#21830,#5201);
#3911=LINE('',#21832,#5202);
#3912=LINE('',#21833,#5203);
#3913=LINE('',#21836,#5204);
#3914=LINE('',#21838,#5205);
#3915=LINE('',#21839,#5206);
#3916=LINE('',#21842,#5207);
#3917=LINE('',#21844,#5208);
#3918=LINE('',#21845,#5209);
#3919=LINE('',#21848,#5210);
#3920=LINE('',#21850,#5211);
#3921=LINE('',#21851,#5212);
#3922=LINE('',#21854,#5213);
#3923=LINE('',#21856,#5214);
#3924=LINE('',#21857,#5215);
#3925=LINE('',#21860,#5216);
#3926=LINE('',#21862,#5217);
#3927=LINE('',#21863,#5218);
#3928=LINE('',#21866,#5219);
#3929=LINE('',#21868,#5220);
#3930=LINE('',#21869,#5221);
#3931=LINE('',#21872,#5222);
#3932=LINE('',#21874,#5223);
#3933=LINE('',#21875,#5224);
#3934=LINE('',#21878,#5225);
#3935=LINE('',#21880,#5226);
#3936=LINE('',#21881,#5227);
#3937=LINE('',#21884,#5228);
#3938=LINE('',#21886,#5229);
#3939=LINE('',#21887,#5230);
#3940=LINE('',#21890,#5231);
#3941=LINE('',#21892,#5232);
#3942=LINE('',#21893,#5233);
#3943=LINE('',#21896,#5234);
#3944=LINE('',#21898,#5235);
#3945=LINE('',#21899,#5236);
#3946=LINE('',#21902,#5237);
#3947=LINE('',#21904,#5238);
#3948=LINE('',#21905,#5239);
#3949=LINE('',#21908,#5240);
#3950=LINE('',#21910,#5241);
#3951=LINE('',#21911,#5242);
#3952=LINE('',#21914,#5243);
#3953=LINE('',#21916,#5244);
#3954=LINE('',#21917,#5245);
#3955=LINE('',#21920,#5246);
#3956=LINE('',#21922,#5247);
#3957=LINE('',#21923,#5248);
#3958=LINE('',#21926,#5249);
#3959=LINE('',#21928,#5250);
#3960=LINE('',#21929,#5251);
#3961=LINE('',#21932,#5252);
#3962=LINE('',#21934,#5253);
#3963=LINE('',#21935,#5254);
#3964=LINE('',#21938,#5255);
#3965=LINE('',#21940,#5256);
#3966=LINE('',#21941,#5257);
#3967=LINE('',#21944,#5258);
#3968=LINE('',#21946,#5259);
#3969=LINE('',#21947,#5260);
#3970=LINE('',#21950,#5261);
#3971=LINE('',#21952,#5262);
#3972=LINE('',#21953,#5263);
#3973=LINE('',#21956,#5264);
#3974=LINE('',#21958,#5265);
#3975=LINE('',#21959,#5266);
#3976=LINE('',#21962,#5267);
#3977=LINE('',#21964,#5268);
#3978=LINE('',#21965,#5269);
#3979=LINE('',#21968,#5270);
#3980=LINE('',#21970,#5271);
#3981=LINE('',#21971,#5272);
#3982=LINE('',#21974,#5273);
#3983=LINE('',#21976,#5274);
#3984=LINE('',#21977,#5275);
#3985=LINE('',#21980,#5276);
#3986=LINE('',#21982,#5277);
#3987=LINE('',#21983,#5278);
#3988=LINE('',#21986,#5279);
#3989=LINE('',#21988,#5280);
#3990=LINE('',#21989,#5281);
#3991=LINE('',#21992,#5282);
#3992=LINE('',#21994,#5283);
#3993=LINE('',#21995,#5284);
#3994=LINE('',#21998,#5285);
#3995=LINE('',#22000,#5286);
#3996=LINE('',#22001,#5287);
#3997=LINE('',#22004,#5288);
#3998=LINE('',#22006,#5289);
#3999=LINE('',#22007,#5290);
#4000=LINE('',#22010,#5291);
#4001=LINE('',#22012,#5292);
#4002=LINE('',#22013,#5293);
#4003=LINE('',#22016,#5294);
#4004=LINE('',#22018,#5295);
#4005=LINE('',#22019,#5296);
#4006=LINE('',#22022,#5297);
#4007=LINE('',#22024,#5298);
#4008=LINE('',#22025,#5299);
#4009=LINE('',#22028,#5300);
#4010=LINE('',#22030,#5301);
#4011=LINE('',#22031,#5302);
#4012=LINE('',#22034,#5303);
#4013=LINE('',#22036,#5304);
#4014=LINE('',#22037,#5305);
#4015=LINE('',#22040,#5306);
#4016=LINE('',#22042,#5307);
#4017=LINE('',#22043,#5308);
#4018=LINE('',#22046,#5309);
#4019=LINE('',#22048,#5310);
#4020=LINE('',#22049,#5311);
#4021=LINE('',#22052,#5312);
#4022=LINE('',#22054,#5313);
#4023=LINE('',#22055,#5314);
#4024=LINE('',#22058,#5315);
#4025=LINE('',#22060,#5316);
#4026=LINE('',#22061,#5317);
#4027=LINE('',#22064,#5318);
#4028=LINE('',#22066,#5319);
#4029=LINE('',#22067,#5320);
#4030=LINE('',#22070,#5321);
#4031=LINE('',#22072,#5322);
#4032=LINE('',#22073,#5323);
#4033=LINE('',#22076,#5324);
#4034=LINE('',#22078,#5325);
#4035=LINE('',#22079,#5326);
#4036=LINE('',#22082,#5327);
#4037=LINE('',#22084,#5328);
#4038=LINE('',#22085,#5329);
#4039=LINE('',#22088,#5330);
#4040=LINE('',#22090,#5331);
#4041=LINE('',#22091,#5332);
#4042=LINE('',#22094,#5333);
#4043=LINE('',#22096,#5334);
#4044=LINE('',#22097,#5335);
#4045=LINE('',#22100,#5336);
#4046=LINE('',#22102,#5337);
#4047=LINE('',#22103,#5338);
#4048=LINE('',#22106,#5339);
#4049=LINE('',#22108,#5340);
#4050=LINE('',#22109,#5341);
#4051=LINE('',#22112,#5342);
#4052=LINE('',#22114,#5343);
#4053=LINE('',#22115,#5344);
#4054=LINE('',#22118,#5345);
#4055=LINE('',#22120,#5346);
#4056=LINE('',#22121,#5347);
#4057=LINE('',#22124,#5348);
#4058=LINE('',#22126,#5349);
#4059=LINE('',#22127,#5350);
#4060=LINE('',#22130,#5351);
#4061=LINE('',#22132,#5352);
#4062=LINE('',#22133,#5353);
#4063=LINE('',#22136,#5354);
#4064=LINE('',#22138,#5355);
#4065=LINE('',#22139,#5356);
#4066=LINE('',#22142,#5357);
#4067=LINE('',#22144,#5358);
#4068=LINE('',#22145,#5359);
#4069=LINE('',#22148,#5360);
#4070=LINE('',#22150,#5361);
#4071=LINE('',#22151,#5362);
#4072=LINE('',#22154,#5363);
#4073=LINE('',#22156,#5364);
#4074=LINE('',#22157,#5365);
#4075=LINE('',#22160,#5366);
#4076=LINE('',#22162,#5367);
#4077=LINE('',#22163,#5368);
#4078=LINE('',#22166,#5369);
#4079=LINE('',#22168,#5370);
#4080=LINE('',#22169,#5371);
#4081=LINE('',#22172,#5372);
#4082=LINE('',#22174,#5373);
#4083=LINE('',#22175,#5374);
#4084=LINE('',#22178,#5375);
#4085=LINE('',#22180,#5376);
#4086=LINE('',#22181,#5377);
#4087=LINE('',#22184,#5378);
#4088=LINE('',#22186,#5379);
#4089=LINE('',#22187,#5380);
#4090=LINE('',#22190,#5381);
#4091=LINE('',#22192,#5382);
#4092=LINE('',#22193,#5383);
#4093=LINE('',#22196,#5384);
#4094=LINE('',#22198,#5385);
#4095=LINE('',#22199,#5386);
#4096=LINE('',#22202,#5387);
#4097=LINE('',#22204,#5388);
#4098=LINE('',#22205,#5389);
#4099=LINE('',#22208,#5390);
#4100=LINE('',#22210,#5391);
#4101=LINE('',#22211,#5392);
#4102=LINE('',#22214,#5393);
#4103=LINE('',#22216,#5394);
#4104=LINE('',#22217,#5395);
#4105=LINE('',#22220,#5396);
#4106=LINE('',#22222,#5397);
#4107=LINE('',#22223,#5398);
#4108=LINE('',#22226,#5399);
#4109=LINE('',#22228,#5400);
#4110=LINE('',#22229,#5401);
#4111=LINE('',#22232,#5402);
#4112=LINE('',#22234,#5403);
#4113=LINE('',#22235,#5404);
#4114=LINE('',#22238,#5405);
#4115=LINE('',#22240,#5406);
#4116=LINE('',#22241,#5407);
#4117=LINE('',#22244,#5408);
#4118=LINE('',#22246,#5409);
#4119=LINE('',#22247,#5410);
#4120=LINE('',#22249,#5411);
#4121=LINE('',#22250,#5412);
#4122=LINE('',#22258,#5413);
#4123=LINE('',#22262,#5414);
#4124=LINE('',#22266,#5415);
#4125=LINE('',#22270,#5416);
#4126=LINE('',#22274,#5417);
#4127=LINE('',#22278,#5418);
#4128=LINE('',#22282,#5419);
#4129=LINE('',#22286,#5420);
#4130=LINE('',#22290,#5421);
#4131=LINE('',#22294,#5422);
#4132=LINE('',#22298,#5423);
#4133=LINE('',#22302,#5424);
#4134=LINE('',#22306,#5425);
#4135=LINE('',#22310,#5426);
#4136=LINE('',#22314,#5427);
#4137=LINE('',#22318,#5428);
#4138=LINE('',#22320,#5429);
#4139=LINE('',#22322,#5430);
#4140=LINE('',#22324,#5431);
#4141=LINE('',#22326,#5432);
#4142=LINE('',#22328,#5433);
#4143=LINE('',#22329,#5434);
#4144=LINE('',#22331,#5435);
#4145=LINE('',#22333,#5436);
#4146=LINE('',#22335,#5437);
#4147=LINE('',#22337,#5438);
#4148=LINE('',#22339,#5439);
#4149=LINE('',#22340,#5440);
#4150=LINE('',#22343,#5441);
#4151=LINE('',#22345,#5442);
#4152=LINE('',#22347,#5443);
#4153=LINE('',#22349,#5444);
#4154=LINE('',#22350,#5445);
#4155=LINE('',#22352,#5446);
#4156=LINE('',#22354,#5447);
#4157=LINE('',#22356,#5448);
#4158=LINE('',#22358,#5449);
#4159=LINE('',#22359,#5450);
#4160=LINE('',#22362,#5451);
#4161=LINE('',#22363,#5452);
#4162=LINE('',#22366,#5453);
#4163=LINE('',#22367,#5454);
#4164=LINE('',#22370,#5455);
#4165=LINE('',#22371,#5456);
#4166=LINE('',#22374,#5457);
#4167=LINE('',#22375,#5458);
#4168=LINE('',#22377,#5459);
#4169=LINE('',#22380,#5460);
#4170=LINE('',#22381,#5461);
#4171=LINE('',#22384,#5462);
#4172=LINE('',#22385,#5463);
#4173=LINE('',#22388,#5464);
#4174=LINE('',#22389,#5465);
#4175=LINE('',#22392,#5466);
#4176=LINE('',#22393,#5467);
#4177=LINE('',#22395,#5468);
#4178=LINE('',#22401,#5469);
#4179=LINE('',#22403,#5470);
#4180=LINE('',#22405,#5471);
#4181=LINE('',#22406,#5472);
#4182=LINE('',#22409,#5473);
#4183=LINE('',#22411,#5474);
#4184=LINE('',#22412,#5475);
#4185=LINE('',#22415,#5476);
#4186=LINE('',#22417,#5477);
#4187=LINE('',#22418,#5478);
#4188=LINE('',#22421,#5479);
#4189=LINE('',#22423,#5480);
#4190=LINE('',#22424,#5481);
#4191=LINE('',#22427,#5482);
#4192=LINE('',#22429,#5483);
#4193=LINE('',#22430,#5484);
#4194=LINE('',#22433,#5485);
#4195=LINE('',#22435,#5486);
#4196=LINE('',#22436,#5487);
#4197=LINE('',#22439,#5488);
#4198=LINE('',#22441,#5489);
#4199=LINE('',#22442,#5490);
#4200=LINE('',#22444,#5491);
#4201=LINE('',#22445,#5492);
#4202=LINE('',#22452,#5493);
#4203=LINE('',#22454,#5494);
#4204=LINE('',#22456,#5495);
#4205=LINE('',#22457,#5496);
#4206=LINE('',#22460,#5497);
#4207=LINE('',#22462,#5498);
#4208=LINE('',#22463,#5499);
#4209=LINE('',#22466,#5500);
#4210=LINE('',#22468,#5501);
#4211=LINE('',#22469,#5502);
#4212=LINE('',#22472,#5503);
#4213=LINE('',#22474,#5504);
#4214=LINE('',#22475,#5505);
#4215=LINE('',#22478,#5506);
#4216=LINE('',#22480,#5507);
#4217=LINE('',#22481,#5508);
#4218=LINE('',#22484,#5509);
#4219=LINE('',#22486,#5510);
#4220=LINE('',#22487,#5511);
#4221=LINE('',#22490,#5512);
#4222=LINE('',#22492,#5513);
#4223=LINE('',#22493,#5514);
#4224=LINE('',#22495,#5515);
#4225=LINE('',#22496,#5516);
#4226=LINE('',#22506,#5517);
#4227=LINE('',#22508,#5518);
#4228=LINE('',#22510,#5519);
#4229=LINE('',#22511,#5520);
#4230=LINE('',#22514,#5521);
#4231=LINE('',#22516,#5522);
#4232=LINE('',#22517,#5523);
#4233=LINE('',#22520,#5524);
#4234=LINE('',#22522,#5525);
#4235=LINE('',#22523,#5526);
#4236=LINE('',#22526,#5527);
#4237=LINE('',#22528,#5528);
#4238=LINE('',#22529,#5529);
#4239=LINE('',#22532,#5530);
#4240=LINE('',#22534,#5531);
#4241=LINE('',#22535,#5532);
#4242=LINE('',#22537,#5533);
#4243=LINE('',#22538,#5534);
#4244=LINE('',#22550,#5535);
#4245=LINE('',#22554,#5536);
#4246=LINE('',#22558,#5537);
#4247=LINE('',#22565,#5538);
#4248=LINE('',#22567,#5539);
#4249=LINE('',#22573,#5540);
#4250=LINE('',#22575,#5541);
#4251=LINE('',#22577,#5542);
#4252=LINE('',#22578,#5543);
#4253=LINE('',#22583,#5544);
#4254=LINE('',#22584,#5545);
#4255=LINE('',#22587,#5546);
#4256=LINE('',#22589,#5547);
#4257=LINE('',#22590,#5548);
#4258=LINE('',#22592,#5549);
#4259=LINE('',#22599,#5550);
#4260=LINE('',#22606,#5551);
#4261=LINE('',#22612,#5552);
#4262=LINE('',#22614,#5553);
#4263=LINE('',#22616,#5554);
#4264=LINE('',#22617,#5555);
#4265=LINE('',#22622,#5556);
#4266=LINE('',#22623,#5557);
#4267=LINE('',#22626,#5558);
#4268=LINE('',#22628,#5559);
#4269=LINE('',#22629,#5560);
#4270=LINE('',#22631,#5561);
#4271=LINE('',#22645,#5562);
#4272=LINE('',#22648,#5563);
#4273=LINE('',#22653,#5564);
#4274=LINE('',#22661,#5565);
#4275=LINE('',#22667,#5566);
#4276=LINE('',#22676,#5567);
#4277=LINE('',#22682,#5568);
#4278=LINE('',#22691,#5569);
#4279=LINE('',#22697,#5570);
#4280=LINE('',#22706,#5571);
#4281=LINE('',#22712,#5572);
#4282=LINE('',#22721,#5573);
#4283=LINE('',#22727,#5574);
#4284=LINE('',#22736,#5575);
#4285=LINE('',#22742,#5576);
#4286=LINE('',#22751,#5577);
#4287=LINE('',#22756,#5578);
#4288=LINE('',#22758,#5579);
#4289=LINE('',#22760,#5580);
#4290=LINE('',#22761,#5581);
#4291=LINE('',#22764,#5582);
#4292=LINE('',#22766,#5583);
#4293=LINE('',#22767,#5584);
#4294=LINE('',#22770,#5585);
#4295=LINE('',#22772,#5586);
#4296=LINE('',#22773,#5587);
#4297=LINE('',#22783,#5588);
#4298=LINE('',#22787,#5589);
#4299=LINE('',#22791,#5590);
#4300=LINE('',#22793,#5591);
#4301=LINE('',#22794,#5592);
#4302=LINE('',#22797,#5593);
#4303=LINE('',#22801,#5594);
#4304=LINE('',#22802,#5595);
#4305=LINE('',#22807,#5596);
#4306=LINE('',#22815,#5597);
#4307=LINE('',#22821,#5598);
#4308=LINE('',#22829,#5599);
#4309=LINE('',#22831,#5600);
#4310=LINE('',#22833,#5601);
#4311=LINE('',#22834,#5602);
#4312=LINE('',#22837,#5603);
#4313=LINE('',#22839,#5604);
#4314=LINE('',#22840,#5605);
#4315=LINE('',#22843,#5606);
#4316=LINE('',#22845,#5607);
#4317=LINE('',#22846,#5608);
#4318=LINE('',#22923,#5609);
#4319=LINE('',#23069,#5610);
#4320=LINE('',#23215,#5611);
#4321=LINE('',#23361,#5612);
#4322=LINE('',#23507,#5613);
#4323=LINE('',#23653,#5614);
#4324=LINE('',#23799,#5615);
#4325=LINE('',#23945,#5616);
#4326=LINE('',#24091,#5617);
#4327=LINE('',#24237,#5618);
#4328=LINE('',#24383,#5619);
#4329=LINE('',#24529,#5620);
#4330=LINE('',#24675,#5621);
#4331=LINE('',#24821,#5622);
#4332=LINE('',#24967,#5623);
#4333=LINE('',#25113,#5624);
#4334=LINE('',#25259,#5625);
#4335=LINE('',#25405,#5626);
#4336=LINE('',#25551,#5627);
#4337=LINE('',#25697,#5628);
#4338=LINE('',#25775,#5629);
#4339=LINE('',#25919,#5630);
#4340=LINE('',#25991,#5631);
#4341=LINE('',#25994,#5632);
#4342=LINE('',#25995,#5633);
#4343=LINE('',#26207,#5634);
#4344=LINE('',#26211,#5635);
#4345=LINE('',#26423,#5636);
#4346=LINE('',#26426,#5637);
#4347=LINE('',#26427,#5638);
#4348=LINE('',#26639,#5639);
#4349=LINE('',#26643,#5640);
#4350=LINE('',#26855,#5641);
#4351=LINE('',#26858,#5642);
#4352=LINE('',#26859,#5643);
#4353=LINE('',#27071,#5644);
#4354=LINE('',#27075,#5645);
#4355=LINE('',#27287,#5646);
#4356=LINE('',#27290,#5647);
#4357=LINE('',#27291,#5648);
#4358=LINE('',#27503,#5649);
#4359=LINE('',#27507,#5650);
#4360=LINE('',#27719,#5651);
#4361=LINE('',#27722,#5652);
#4362=LINE('',#27723,#5653);
#4363=LINE('',#27935,#5654);
#4364=LINE('',#27939,#5655);
#4365=LINE('',#28151,#5656);
#4366=LINE('',#28154,#5657);
#4367=LINE('',#28155,#5658);
#4368=LINE('',#28367,#5659);
#4369=LINE('',#28371,#5660);
#4370=LINE('',#28583,#5661);
#4371=LINE('',#28586,#5662);
#4372=LINE('',#28587,#5663);
#4373=LINE('',#28799,#5664);
#4374=LINE('',#28803,#5665);
#4375=LINE('',#29015,#5666);
#4376=LINE('',#29018,#5667);
#4377=LINE('',#29019,#5668);
#4378=LINE('',#29231,#5669);
#4379=LINE('',#29235,#5670);
#4380=LINE('',#29447,#5671);
#4381=LINE('',#29450,#5672);
#4382=LINE('',#29451,#5673);
#4383=LINE('',#29663,#5674);
#4384=LINE('',#29667,#5675);
#4385=LINE('',#29879,#5676);
#4386=LINE('',#29882,#5677);
#4387=LINE('',#29883,#5678);
#4388=LINE('',#30095,#5679);
#4389=LINE('',#30099,#5680);
#4390=LINE('',#30311,#5681);
#4391=LINE('',#30314,#5682);
#4392=LINE('',#30315,#5683);
#4393=LINE('',#30527,#5684);
#4394=LINE('',#30531,#5685);
#4395=LINE('',#30743,#5686);
#4396=LINE('',#30746,#5687);
#4397=LINE('',#30747,#5688);
#4398=LINE('',#30959,#5689);
#4399=LINE('',#30963,#5690);
#4400=LINE('',#31175,#5691);
#4401=LINE('',#31178,#5692);
#4402=LINE('',#31179,#5693);
#4403=LINE('',#31391,#5694);
#4404=LINE('',#31395,#5695);
#4405=LINE('',#31607,#5696);
#4406=LINE('',#31610,#5697);
#4407=LINE('',#31611,#5698);
#4408=LINE('',#31823,#5699);
#4409=LINE('',#31827,#5700);
#4410=LINE('',#32039,#5701);
#4411=LINE('',#32042,#5702);
#4412=LINE('',#32043,#5703);
#4413=LINE('',#32255,#5704);
#4414=LINE('',#32259,#5705);
#4415=LINE('',#32471,#5706);
#4416=LINE('',#32474,#5707);
#4417=LINE('',#32475,#5708);
#4418=LINE('',#32687,#5709);
#4419=LINE('',#32691,#5710);
#4420=LINE('',#32903,#5711);
#4421=LINE('',#32906,#5712);
#4422=LINE('',#32907,#5713);
#4423=LINE('',#33119,#5714);
#4424=LINE('',#33123,#5715);
#4425=LINE('',#33335,#5716);
#4426=LINE('',#33338,#5717);
#4427=LINE('',#33339,#5718);
#4428=LINE('',#33551,#5719);
#4429=LINE('',#33555,#5720);
#4430=LINE('',#33767,#5721);
#4431=LINE('',#33770,#5722);
#4432=LINE('',#33771,#5723);
#4433=LINE('',#33983,#5724);
#4434=LINE('',#33987,#5725);
#4435=LINE('',#34199,#5726);
#4436=LINE('',#34202,#5727);
#4437=LINE('',#34203,#5728);
#4438=LINE('',#34415,#5729);
#4439=LINE('',#34426,#5730);
#4440=LINE('',#34430,#5731);
#4441=LINE('',#34434,#5732);
#4442=LINE('',#34441,#5733);
#4443=LINE('',#34445,#5734);
#4444=LINE('',#34449,#5735);
#4445=LINE('',#34454,#5736);
#4446=LINE('',#34456,#5737);
#4447=LINE('',#34458,#5738);
#4448=LINE('',#34459,#5739);
#4449=LINE('',#34462,#5740);
#4450=LINE('',#34464,#5741);
#4451=LINE('',#34465,#5742);
#4452=LINE('',#34468,#5743);
#4453=LINE('',#34470,#5744);
#4454=LINE('',#34471,#5745);
#4455=LINE('',#34474,#5746);
#4456=LINE('',#34476,#5747);
#4457=LINE('',#34477,#5748);
#4458=LINE('',#34480,#5749);
#4459=LINE('',#34482,#5750);
#4460=LINE('',#34483,#5751);
#4461=LINE('',#34485,#5752);
#4462=LINE('',#34486,#5753);
#4463=LINE('',#34575,#5754);
#4464=LINE('',#34577,#5755);
#4465=LINE('',#34579,#5756);
#4466=LINE('',#34581,#5757);
#4467=LINE('',#34583,#5758);
#4468=LINE('',#34585,#5759);
#4469=LINE('',#34587,#5760);
#4470=LINE('',#34588,#5761);
#4471=LINE('',#34591,#5762);
#4472=LINE('',#34593,#5763);
#4473=LINE('',#34594,#5764);
#4474=LINE('',#34597,#5765);
#4475=LINE('',#34598,#5766);
#4476=LINE('',#34601,#5767);
#4477=LINE('',#34602,#5768);
#4478=LINE('',#34605,#5769);
#4479=LINE('',#34606,#5770);
#4480=LINE('',#34609,#5771);
#4481=LINE('',#34611,#5772);
#4482=LINE('',#34613,#5773);
#4483=LINE('',#34614,#5774);
#4484=LINE('',#34616,#5775);
#4485=LINE('',#34618,#5776);
#4486=LINE('',#34620,#5777);
#4487=LINE('',#34627,#5778);
#4488=LINE('',#34633,#5779);
#4489=LINE('',#34644,#5780);
#4490=LINE('',#34648,#5781);
#4491=LINE('',#34652,#5782);
#4492=LINE('',#34659,#5783);
#4493=LINE('',#34663,#5784);
#4494=LINE('',#34667,#5785);
#4495=LINE('',#34672,#5786);
#4496=LINE('',#34674,#5787);
#4497=LINE('',#34676,#5788);
#4498=LINE('',#34677,#5789);
#4499=LINE('',#34680,#5790);
#4500=LINE('',#34682,#5791);
#4501=LINE('',#34683,#5792);
#4502=LINE('',#34686,#5793);
#4503=LINE('',#34688,#5794);
#4504=LINE('',#34689,#5795);
#4505=LINE('',#34692,#5796);
#4506=LINE('',#34694,#5797);
#4507=LINE('',#34695,#5798);
#4508=LINE('',#34698,#5799);
#4509=LINE('',#34700,#5800);
#4510=LINE('',#34701,#5801);
#4511=LINE('',#34703,#5802);
#4512=LINE('',#34704,#5803);
#4513=LINE('',#34729,#5804);
#4514=LINE('',#34735,#5805);
#4515=VECTOR('',#15610,0.274999999999999);
#4516=VECTOR('',#15617,0.274999999999999);
#4517=VECTOR('',#15624,0.275);
#4518=VECTOR('',#15631,0.275);
#4519=VECTOR('',#15636,1.);
#4520=VECTOR('',#15637,1.);
#4521=VECTOR('',#15638,1.);
#4522=VECTOR('',#15639,1.);
#4523=VECTOR('',#15642,1.);
#4524=VECTOR('',#15643,1.);
#4525=VECTOR('',#15644,1.);
#4526=VECTOR('',#15647,1.);
#4527=VECTOR('',#15648,1.);
#4528=VECTOR('',#15649,1.);
#4529=VECTOR('',#15652,1.);
#4530=VECTOR('',#15653,1.);
#4531=VECTOR('',#15662,1.);
#4532=VECTOR('',#15663,1.);
#4533=VECTOR('',#15664,1.);
#4534=VECTOR('',#15665,1.);
#4535=VECTOR('',#15668,1.);
#4536=VECTOR('',#15669,1.);
#4537=VECTOR('',#15670,1.);
#4538=VECTOR('',#15673,1.);
#4539=VECTOR('',#15674,1.);
#4540=VECTOR('',#15675,1.);
#4541=VECTOR('',#15678,1.);
#4542=VECTOR('',#15679,1.);
#4543=VECTOR('',#15688,1.);
#4544=VECTOR('',#15689,1.);
#4545=VECTOR('',#15690,1.);
#4546=VECTOR('',#15691,1.);
#4547=VECTOR('',#15694,1.);
#4548=VECTOR('',#15695,1.);
#4549=VECTOR('',#15696,1.);
#4550=VECTOR('',#15699,1.);
#4551=VECTOR('',#15700,1.);
#4552=VECTOR('',#15701,1.);
#4553=VECTOR('',#15704,1.);
#4554=VECTOR('',#15705,1.);
#4555=VECTOR('',#15716,0.164999999999999);
#4556=VECTOR('',#15723,0.164999999999999);
#4557=VECTOR('',#15730,0.164999999999999);
#4558=VECTOR('',#15737,0.164999999999999);
#4559=VECTOR('',#15744,0.210000000000001);
#4560=VECTOR('',#15751,0.210000000000001);
#4561=VECTOR('',#15758,0.21);
#4562=VECTOR('',#15765,0.21);
#4563=VECTOR('',#15772,0.164999999999999);
#4564=VECTOR('',#15779,0.164999999999999);
#4565=VECTOR('',#15786,0.165);
#4566=VECTOR('',#15793,0.164999999999999);
#4567=VECTOR('',#15800,0.274999999999999);
#4568=VECTOR('',#15807,0.274999999999999);
#4569=VECTOR('',#15814,0.275);
#4570=VECTOR('',#15821,0.275);
#4571=VECTOR('',#15826,1.);
#4572=VECTOR('',#15827,1.);
#4573=VECTOR('',#15828,1.);
#4574=VECTOR('',#15829,1.);
#4575=VECTOR('',#15832,1.);
#4576=VECTOR('',#15833,1.);
#4577=VECTOR('',#15834,1.);
#4578=VECTOR('',#15837,1.);
#4579=VECTOR('',#15838,1.);
#4580=VECTOR('',#15839,1.);
#4581=VECTOR('',#15842,1.);
#4582=VECTOR('',#15843,1.);
#4583=VECTOR('',#15854,0.5);
#4584=VECTOR('',#15865,0.5);
#4585=VECTOR('',#15876,0.275);
#4586=VECTOR('',#15881,0.275);
#4587=VECTOR('',#15884,1.);
#4588=VECTOR('',#15885,1.);
#4589=VECTOR('',#15886,1.);
#4590=VECTOR('',#15887,1.);
#4591=VECTOR('',#15890,1.);
#4592=VECTOR('',#15891,1.);
#4593=VECTOR('',#15892,1.);
#4594=VECTOR('',#15895,1.);
#4595=VECTOR('',#15896,1.);
#4596=VECTOR('',#15897,1.);
#4597=VECTOR('',#15900,1.);
#4598=VECTOR('',#15901,1.);
#4599=VECTOR('',#15910,1.);
#4600=VECTOR('',#15911,1.);
#4601=VECTOR('',#15912,1.);
#4602=VECTOR('',#15913,1.);
#4603=VECTOR('',#15916,1.);
#4604=VECTOR('',#15917,1.);
#4605=VECTOR('',#15918,1.);
#4606=VECTOR('',#15921,1.);
#4607=VECTOR('',#15922,1.);
#4608=VECTOR('',#15923,1.);
#4609=VECTOR('',#15926,1.);
#4610=VECTOR('',#15927,1.);
#4611=VECTOR('',#15938,0.5);
#4612=VECTOR('',#15949,0.5);
#4613=VECTOR('',#15960,0.274999999999999);
#4614=VECTOR('',#15965,0.274999999999999);
#4615=VECTOR('',#15968,1.);
#4616=VECTOR('',#15969,1.);
#4617=VECTOR('',#15970,1.);
#4618=VECTOR('',#15971,1.);
#4619=VECTOR('',#15974,1.);
#4620=VECTOR('',#15975,1.);
#4621=VECTOR('',#15976,1.);
#4622=VECTOR('',#15979,1.);
#4623=VECTOR('',#15980,1.);
#4624=VECTOR('',#15981,1.);
#4625=VECTOR('',#15984,1.);
#4626=VECTOR('',#15985,1.);
#4627=VECTOR('',#15994,1.);
#4628=VECTOR('',#15995,1.);
#4629=VECTOR('',#15996,1.);
#4630=VECTOR('',#15997,1.);
#4631=VECTOR('',#16000,1.);
#4632=VECTOR('',#16001,1.);
#4633=VECTOR('',#16002,1.);
#4634=VECTOR('',#16005,1.);
#4635=VECTOR('',#16006,1.);
#4636=VECTOR('',#16007,1.);
#4637=VECTOR('',#16010,1.);
#4638=VECTOR('',#16011,1.);
#4639=VECTOR('',#16022,0.225);
#4640=VECTOR('',#16029,0.225);
#4641=VECTOR('',#16036,0.164999999999999);
#4642=VECTOR('',#16043,0.164999999999999);
#4643=VECTOR('',#16050,0.164999999999999);
#4644=VECTOR('',#16057,0.164999999999999);
#4645=VECTOR('',#16064,1.6);
#4646=VECTOR('',#16069,1.);
#4647=VECTOR('',#16070,1.);
#4648=VECTOR('',#16071,1.);
#4649=VECTOR('',#16072,1.);
#4650=VECTOR('',#16075,1.);
#4651=VECTOR('',#16076,1.);
#4652=VECTOR('',#16077,1.);
#4653=VECTOR('',#16078,1.);
#4654=VECTOR('',#16081,1.);
#4655=VECTOR('',#16082,1.);
#4656=VECTOR('',#16083,1.);
#4657=VECTOR('',#16086,1.);
#4658=VECTOR('',#16087,1.);
#4659=VECTOR('',#16088,1.);
#4660=VECTOR('',#16091,1.);
#4661=VECTOR('',#16092,1.);
#4662=VECTOR('',#16093,1.);
#4663=VECTOR('',#16094,1.);
#4664=VECTOR('',#16097,1.);
#4665=VECTOR('',#16098,1.);
#4666=VECTOR('',#16101,1.);
#4667=VECTOR('',#16102,1.);
#4668=VECTOR('',#16103,1.);
#4669=VECTOR('',#16106,1.);
#4670=VECTOR('',#16117,0.225);
#4671=VECTOR('',#16124,0.225);
#4672=VECTOR('',#16131,0.225);
#4673=VECTOR('',#16138,0.225);
#4674=VECTOR('',#16145,1.59);
#4675=VECTOR('',#16154,1.2);
#4676=VECTOR('',#16161,2.4);
#4677=VECTOR('',#16174,0.225);
#4678=VECTOR('',#16181,0.225);
#4679=VECTOR('',#16188,0.225);
#4680=VECTOR('',#16195,0.225);
#4681=VECTOR('',#16202,1.59);
#4682=VECTOR('',#16213,1.2);
#4683=VECTOR('',#16218,2.4);
#4684=VECTOR('',#16231,0.225);
#4685=VECTOR('',#16238,0.225);
#4686=VECTOR('',#16245,0.164999999999999);
#4687=VECTOR('',#16252,0.164999999999999);
#4688=VECTOR('',#16259,0.164999999999999);
#4689=VECTOR('',#16266,0.164999999999999);
#4690=VECTOR('',#16273,1.6);
#4691=VECTOR('',#16278,1.);
#4692=VECTOR('',#16279,1.);
#4693=VECTOR('',#16280,1.);
#4694=VECTOR('',#16281,1.);
#4695=VECTOR('',#16284,1.);
#4696=VECTOR('',#16285,1.);
#4697=VECTOR('',#16286,1.);
#4698=VECTOR('',#16287,1.);
#4699=VECTOR('',#16290,1.);
#4700=VECTOR('',#16291,1.);
#4701=VECTOR('',#16292,1.);
#4702=VECTOR('',#16295,1.);
#4703=VECTOR('',#16296,1.);
#4704=VECTOR('',#16297,1.);
#4705=VECTOR('',#16300,1.);
#4706=VECTOR('',#16301,1.);
#4707=VECTOR('',#16302,1.);
#4708=VECTOR('',#16303,1.);
#4709=VECTOR('',#16306,1.);
#4710=VECTOR('',#16307,1.);
#4711=VECTOR('',#16310,1.);
#4712=VECTOR('',#16311,1.);
#4713=VECTOR('',#16312,1.);
#4714=VECTOR('',#16315,1.);
#4715=VECTOR('',#16326,0.225);
#4716=VECTOR('',#16333,0.225);
#4717=VECTOR('',#16340,0.225);
#4718=VECTOR('',#16347,0.225);
#4719=VECTOR('',#16354,1.59);
#4720=VECTOR('',#16363,1.2);
#4721=VECTOR('',#16370,2.4);
#4722=VECTOR('',#16383,0.225);
#4723=VECTOR('',#16390,0.225);
#4724=VECTOR('',#16397,0.225);
#4725=VECTOR('',#16404,0.225);
#4726=VECTOR('',#16411,1.59);
#4727=VECTOR('',#16422,1.2);
#4728=VECTOR('',#16427,2.4);
#4729=VECTOR('',#16438,1.);
#4730=VECTOR('',#16439,1.);
#4731=VECTOR('',#16440,1.);
#4732=VECTOR('',#16441,1.);
#4733=VECTOR('',#16444,1.);
#4734=VECTOR('',#16445,1.);
#4735=VECTOR('',#16446,1.);
#4736=VECTOR('',#16449,1.);
#4737=VECTOR('',#16450,1.);
#4738=VECTOR('',#16451,1.);
#4739=VECTOR('',#16454,1.);
#4740=VECTOR('',#16455,1.);
#4741=VECTOR('',#16456,1.);
#4742=VECTOR('',#16459,1.);
#4743=VECTOR('',#16460,1.);
#4744=VECTOR('',#16461,1.);
#4745=VECTOR('',#16464,1.);
#4746=VECTOR('',#16465,1.);
#4747=VECTOR('',#16466,1.);
#4748=VECTOR('',#16469,1.);
#4749=VECTOR('',#16470,1.);
#4750=VECTOR('',#16471,1.);
#4751=VECTOR('',#16474,1.);
#4752=VECTOR('',#16475,1.);
#4753=VECTOR('',#16476,1.);
#4754=VECTOR('',#16479,1.);
#4755=VECTOR('',#16480,1.);
#4756=VECTOR('',#16481,1.);
#4757=VECTOR('',#16484,1.);
#4758=VECTOR('',#16485,1.);
#4759=VECTOR('',#16486,1.);
#4760=VECTOR('',#16487,1.);
#4761=VECTOR('',#16490,1.);
#4762=VECTOR('',#16491,1.);
#4763=VECTOR('',#16492,1.);
#4764=VECTOR('',#16495,1.);
#4765=VECTOR('',#16496,1.);
#4766=VECTOR('',#16497,1.);
#4767=VECTOR('',#16500,1.);
#4768=VECTOR('',#16501,1.);
#4769=VECTOR('',#16502,1.);
#4770=VECTOR('',#16505,1.);
#4771=VECTOR('',#16506,1.);
#4772=VECTOR('',#16507,1.);
#4773=VECTOR('',#16510,1.);
#4774=VECTOR('',#16511,1.);
#4775=VECTOR('',#16512,1.);
#4776=VECTOR('',#16515,1.);
#4777=VECTOR('',#16516,1.);
#4778=VECTOR('',#16517,1.);
#4779=VECTOR('',#16520,1.);
#4780=VECTOR('',#16521,1.);
#4781=VECTOR('',#16522,1.);
#4782=VECTOR('',#16525,1.);
#4783=VECTOR('',#16526,1.);
#4784=VECTOR('',#16527,1.);
#4785=VECTOR('',#16530,1.);
#4786=VECTOR('',#16531,1.);
#4787=VECTOR('',#16532,1.);
#4788=VECTOR('',#16533,1.);
#4789=VECTOR('',#16536,1.);
#4790=VECTOR('',#16537,1.);
#4791=VECTOR('',#16538,1.);
#4792=VECTOR('',#16541,1.);
#4793=VECTOR('',#16542,1.);
#4794=VECTOR('',#16543,1.);
#4795=VECTOR('',#16546,1.);
#4796=VECTOR('',#16547,1.);
#4797=VECTOR('',#16548,1.);
#4798=VECTOR('',#16551,1.);
#4799=VECTOR('',#16552,1.);
#4800=VECTOR('',#16553,1.);
#4801=VECTOR('',#16556,1.);
#4802=VECTOR('',#16557,1.);
#4803=VECTOR('',#16558,1.);
#4804=VECTOR('',#16561,1.);
#4805=VECTOR('',#16562,1.);
#4806=VECTOR('',#16563,1.);
#4807=VECTOR('',#16566,1.);
#4808=VECTOR('',#16567,1.);
#4809=VECTOR('',#16568,1.);
#4810=VECTOR('',#16571,1.);
#4811=VECTOR('',#16572,1.);
#4812=VECTOR('',#16573,1.);
#4813=VECTOR('',#16576,1.);
#4814=VECTOR('',#16577,1.);
#4815=VECTOR('',#16578,1.);
#4816=VECTOR('',#16579,1.);
#4817=VECTOR('',#16582,1.);
#4818=VECTOR('',#16583,1.);
#4819=VECTOR('',#16584,1.);
#4820=VECTOR('',#16587,1.);
#4821=VECTOR('',#16588,1.);
#4822=VECTOR('',#16589,1.);
#4823=VECTOR('',#16592,1.);
#4824=VECTOR('',#16593,1.);
#4825=VECTOR('',#16594,1.);
#4826=VECTOR('',#16597,1.);
#4827=VECTOR('',#16598,1.);
#4828=VECTOR('',#16599,1.);
#4829=VECTOR('',#16602,1.);
#4830=VECTOR('',#16603,1.);
#4831=VECTOR('',#16604,1.);
#4832=VECTOR('',#16607,1.);
#4833=VECTOR('',#16608,1.);
#4834=VECTOR('',#16609,1.);
#4835=VECTOR('',#16612,1.);
#4836=VECTOR('',#16613,1.);
#4837=VECTOR('',#16614,1.);
#4838=VECTOR('',#16617,1.);
#4839=VECTOR('',#16618,1.);
#4840=VECTOR('',#16619,1.);
#4841=VECTOR('',#16624,0.21);
#4842=VECTOR('',#16629,1.);
#4843=VECTOR('',#16630,1.);
#4844=VECTOR('',#16631,1.);
#4845=VECTOR('',#16634,1.);
#4846=VECTOR('',#16635,1.);
#4847=VECTOR('',#16636,1.);
#4848=VECTOR('',#16639,1.);
#4849=VECTOR('',#16640,1.);
#4850=VECTOR('',#16643,1.);
#4851=VECTOR('',#16644,1.);
#4852=VECTOR('',#16645,1.);
#4853=VECTOR('',#16648,1.);
#4854=VECTOR('',#16649,1.);
#4855=VECTOR('',#16652,1.);
#4856=VECTOR('',#16653,1.);
#4857=VECTOR('',#16654,1.);
#4858=VECTOR('',#16657,1.);
#4859=VECTOR('',#16658,1.);
#4860=VECTOR('',#16661,1.);
#4861=VECTOR('',#16662,1.);
#4862=VECTOR('',#16671,1.);
#4863=VECTOR('',#16672,1.);
#4864=VECTOR('',#16673,1.);
#4865=VECTOR('',#16674,1.);
#4866=VECTOR('',#16677,1.);
#4867=VECTOR('',#16678,1.);
#4868=VECTOR('',#16679,1.);
#4869=VECTOR('',#16682,1.);
#4870=VECTOR('',#16683,1.);
#4871=VECTOR('',#16684,1.);
#4872=VECTOR('',#16689,1.);
#4873=VECTOR('',#16690,1.);
#4874=VECTOR('',#16691,1.);
#4875=VECTOR('',#16692,1.);
#4876=VECTOR('',#16693,1.);
#4877=VECTOR('',#16694,1.);
#4878=VECTOR('',#16695,1.);
#4879=VECTOR('',#16698,1.);
#4880=VECTOR('',#16699,1.);
#4881=VECTOR('',#16702,1.);
#4882=VECTOR('',#16703,1.);
#4883=VECTOR('',#16706,1.);
#4884=VECTOR('',#16707,1.);
#4885=VECTOR('',#16708,1.);
#4886=VECTOR('',#16709,1.);
#4887=VECTOR('',#16710,1.);
#4888=VECTOR('',#16713,1.);
#4889=VECTOR('',#16716,1.);
#4890=VECTOR('',#16719,1.);
#4891=VECTOR('',#16724,0.21);
#4892=VECTOR('',#16733,1.);
#4893=VECTOR('',#16736,1.);
#4894=VECTOR('',#16739,1.);
#4895=VECTOR('',#16748,0.275);
#4896=VECTOR('',#16753,0.265);
#4897=VECTOR('',#16762,0.5);
#4898=VECTOR('',#16773,0.375);
#4899=VECTOR('',#16784,0.375);
#4900=VECTOR('',#16795,0.375);
#4901=VECTOR('',#16806,0.375);
#4902=VECTOR('',#16817,0.225);
#4903=VECTOR('',#16822,0.225);
#4904=VECTOR('',#16827,0.225);
#4905=VECTOR('',#16832,0.225000000000001);
#4906=VECTOR('',#16835,1.);
#4907=VECTOR('',#16836,1.);
#4908=VECTOR('',#16837,1.);
#4909=VECTOR('',#16838,1.);
#4910=VECTOR('',#16841,1.);
#4911=VECTOR('',#16842,1.);
#4912=VECTOR('',#16843,1.);
#4913=VECTOR('',#16846,1.);
#4914=VECTOR('',#16847,1.);
#4915=VECTOR('',#16848,1.);
#4916=VECTOR('',#16851,1.);
#4917=VECTOR('',#16852,1.);
#4918=VECTOR('',#16853,1.);
#4919=VECTOR('',#16856,1.);
#4920=VECTOR('',#16857,1.);
#4921=VECTOR('',#16858,1.);
#4922=VECTOR('',#16861,1.);
#4923=VECTOR('',#16862,1.);
#4924=VECTOR('',#16863,1.);
#4925=VECTOR('',#16866,1.);
#4926=VECTOR('',#16867,1.);
#4927=VECTOR('',#16868,1.);
#4928=VECTOR('',#16871,1.);
#4929=VECTOR('',#16872,1.);
#4930=VECTOR('',#16873,1.);
#4931=VECTOR('',#16876,1.);
#4932=VECTOR('',#16877,1.);
#4933=VECTOR('',#16878,1.);
#4934=VECTOR('',#16881,1.);
#4935=VECTOR('',#16882,1.);
#4936=VECTOR('',#16883,1.);
#4937=VECTOR('',#16886,1.);
#4938=VECTOR('',#16887,1.);
#4939=VECTOR('',#16888,1.);
#4940=VECTOR('',#16891,1.);
#4941=VECTOR('',#16892,1.);
#4942=VECTOR('',#16907,0.4);
#4943=VECTOR('',#16912,0.425);
#4944=VECTOR('',#16917,0.41);
#4945=VECTOR('',#16926,0.26);
#4946=VECTOR('',#16931,0.25);
#4947=VECTOR('',#16936,0.225);
#4948=VECTOR('',#16941,1.);
#4949=VECTOR('',#16942,1.);
#4950=VECTOR('',#16943,1.);
#4951=VECTOR('',#16944,1.);
#4952=VECTOR('',#16947,1.);
#4953=VECTOR('',#16948,1.);
#4954=VECTOR('',#16949,1.);
#4955=VECTOR('',#16952,1.);
#4956=VECTOR('',#16953,1.);
#4957=VECTOR('',#16954,1.);
#4958=VECTOR('',#16957,1.);
#4959=VECTOR('',#16958,1.);
#4960=VECTOR('',#16959,1.);
#4961=VECTOR('',#16962,1.);
#4962=VECTOR('',#16963,1.);
#4963=VECTOR('',#16964,1.);
#4964=VECTOR('',#16967,1.);
#4965=VECTOR('',#16968,1.);
#4966=VECTOR('',#16991,1.070235);
#4967=VECTOR('',#16998,0.6);
#4968=VECTOR('',#17003,0.63);
#4969=VECTOR('',#17012,1.070235);
#4970=VECTOR('',#17019,0.63);
#4971=VECTOR('',#17038,1.129765);
#4972=VECTOR('',#17049,1.57);
#4973=VECTOR('',#17054,1.6);
#4974=VECTOR('',#17059,1.57);
#4975=VECTOR('',#17064,1.129765);
#4976=VECTOR('',#17111,1.123812);
#4977=VECTOR('',#17180,1.076188);
#4978=VECTOR('',#17209,1.119765);
#4979=VECTOR('',#17216,1.085235);
#4980=VECTOR('',#17227,1.119765);
#4981=VECTOR('',#17234,1.085235);
#4982=VECTOR('',#17249,1.);
#4983=VECTOR('',#17250,1.);
#4984=VECTOR('',#17251,1.);
#4985=VECTOR('',#17252,1.);
#4986=VECTOR('',#17255,1.);
#4987=VECTOR('',#17256,1.);
#4988=VECTOR('',#17257,1.);
#4989=VECTOR('',#17260,1.);
#4990=VECTOR('',#17261,1.);
#4991=VECTOR('',#17262,1.);
#4992=VECTOR('',#17265,1.);
#4993=VECTOR('',#17266,1.);
#4994=VECTOR('',#17267,1.);
#4995=VECTOR('',#17270,1.);
#4996=VECTOR('',#17271,1.);
#4997=VECTOR('',#17272,1.);
#4998=VECTOR('',#17275,1.);
#4999=VECTOR('',#17276,1.);
#5000=VECTOR('',#17293,0.325);
#5001=VECTOR('',#17298,0.35);
#5002=VECTOR('',#17303,0.335);
#5003=VECTOR('',#17312,0.21);
#5004=VECTOR('',#17315,0.2);
#5005=VECTOR('',#17324,0.225000000000001);
#5006=VECTOR('',#17331,0.225);
#5007=VECTOR('',#17338,0.225);
#5008=VECTOR('',#17345,0.225000000000001);
#5009=VECTOR('',#17352,0.275);
#5010=VECTOR('',#17359,0.275);
#5011=VECTOR('',#17366,0.275);
#5012=VECTOR('',#17373,0.275);
#5013=VECTOR('',#17378,1.);
#5014=VECTOR('',#17379,1.);
#5015=VECTOR('',#17380,1.);
#5016=VECTOR('',#17381,1.);
#5017=VECTOR('',#17384,1.);
#5018=VECTOR('',#17385,1.);
#5019=VECTOR('',#17386,1.);
#5020=VECTOR('',#17389,1.);
#5021=VECTOR('',#17390,1.);
#5022=VECTOR('',#17391,1.);
#5023=VECTOR('',#17394,1.);
#5024=VECTOR('',#17395,1.);
#5025=VECTOR('',#17406,0.164999999999999);
#5026=VECTOR('',#17415,0.165);
#5027=VECTOR('',#17424,0.165);
#5028=VECTOR('',#17433,0.164999999999999);
#5029=VECTOR('',#17440,1.);
#5030=VECTOR('',#17441,1.);
#5031=VECTOR('',#17442,1.);
#5032=VECTOR('',#17443,1.);
#5033=VECTOR('',#17446,1.);
#5034=VECTOR('',#17447,1.);
#5035=VECTOR('',#17448,1.);
#5036=VECTOR('',#17451,1.);
#5037=VECTOR('',#17452,1.);
#5038=VECTOR('',#17453,1.);
#5039=VECTOR('',#17456,1.);
#5040=VECTOR('',#17457,1.);
#5041=VECTOR('',#17458,1.);
#5042=VECTOR('',#17461,1.);
#5043=VECTOR('',#17462,1.);
#5044=VECTOR('',#17463,1.);
#5045=VECTOR('',#17466,1.);
#5046=VECTOR('',#17467,1.);
#5047=VECTOR('',#17468,1.);
#5048=VECTOR('',#17471,1.);
#5049=VECTOR('',#17472,1.);
#5050=VECTOR('',#17473,1.);
#5051=VECTOR('',#17476,1.);
#5052=VECTOR('',#17477,1.);
#5053=VECTOR('',#17478,1.);
#5054=VECTOR('',#17481,1.);
#5055=VECTOR('',#17482,1.);
#5056=VECTOR('',#17483,1.);
#5057=VECTOR('',#17486,1.);
#5058=VECTOR('',#17487,1.);
#5059=VECTOR('',#17488,1.);
#5060=VECTOR('',#17491,1.);
#5061=VECTOR('',#17492,1.);
#5062=VECTOR('',#17493,1.);
#5063=VECTOR('',#17496,1.);
#5064=VECTOR('',#17497,1.);
#5065=VECTOR('',#17498,1.);
#5066=VECTOR('',#17501,1.);
#5067=VECTOR('',#17502,1.);
#5068=VECTOR('',#17503,1.);
#5069=VECTOR('',#17506,1.);
#5070=VECTOR('',#17507,1.);
#5071=VECTOR('',#17508,1.);
#5072=VECTOR('',#17511,1.);
#5073=VECTOR('',#17512,1.);
#5074=VECTOR('',#17513,1.);
#5075=VECTOR('',#17516,1.);
#5076=VECTOR('',#17517,1.);
#5077=VECTOR('',#17518,1.);
#5078=VECTOR('',#17521,1.);
#5079=VECTOR('',#17522,1.);
#5080=VECTOR('',#17523,1.);
#5081=VECTOR('',#17526,1.);
#5082=VECTOR('',#17527,1.);
#5083=VECTOR('',#17528,1.);
#5084=VECTOR('',#17531,1.);
#5085=VECTOR('',#17532,1.);
#5086=VECTOR('',#17533,1.);
#5087=VECTOR('',#17536,1.);
#5088=VECTOR('',#17537,1.);
#5089=VECTOR('',#17538,1.);
#5090=VECTOR('',#17541,1.);
#5091=VECTOR('',#17542,1.);
#5092=VECTOR('',#17543,1.);
#5093=VECTOR('',#17546,1.);
#5094=VECTOR('',#17547,1.);
#5095=VECTOR('',#17548,1.);
#5096=VECTOR('',#17551,1.);
#5097=VECTOR('',#17552,1.);
#5098=VECTOR('',#17553,1.);
#5099=VECTOR('',#17556,1.);
#5100=VECTOR('',#17557,1.);
#5101=VECTOR('',#17558,1.);
#5102=VECTOR('',#17561,1.);
#5103=VECTOR('',#17562,1.);
#5104=VECTOR('',#17563,1.);
#5105=VECTOR('',#17566,1.);
#5106=VECTOR('',#17567,1.);
#5107=VECTOR('',#17568,1.);
#5108=VECTOR('',#17571,1.);
#5109=VECTOR('',#17572,1.);
#5110=VECTOR('',#17573,1.);
#5111=VECTOR('',#17576,1.);
#5112=VECTOR('',#17577,1.);
#5113=VECTOR('',#17578,1.);
#5114=VECTOR('',#17581,1.);
#5115=VECTOR('',#17582,1.);
#5116=VECTOR('',#17583,1.);
#5117=VECTOR('',#17586,1.);
#5118=VECTOR('',#17587,1.);
#5119=VECTOR('',#17588,1.);
#5120=VECTOR('',#17591,1.);
#5121=VECTOR('',#17592,1.);
#5122=VECTOR('',#17593,1.);
#5123=VECTOR('',#17596,1.);
#5124=VECTOR('',#17597,1.);
#5125=VECTOR('',#17598,1.);
#5126=VECTOR('',#17601,1.);
#5127=VECTOR('',#17602,1.);
#5128=VECTOR('',#17603,1.);
#5129=VECTOR('',#17606,1.);
#5130=VECTOR('',#17607,1.);
#5131=VECTOR('',#17608,1.);
#5132=VECTOR('',#17611,1.);
#5133=VECTOR('',#17612,1.);
#5134=VECTOR('',#17613,1.);
#5135=VECTOR('',#17616,1.);
#5136=VECTOR('',#17617,1.);
#5137=VECTOR('',#17618,1.);
#5138=VECTOR('',#17621,1.);
#5139=VECTOR('',#17622,1.);
#5140=VECTOR('',#17623,1.);
#5141=VECTOR('',#17626,1.);
#5142=VECTOR('',#17627,1.);
#5143=VECTOR('',#17628,1.);
#5144=VECTOR('',#17631,1.);
#5145=VECTOR('',#17632,1.);
#5146=VECTOR('',#17633,1.);
#5147=VECTOR('',#17636,1.);
#5148=VECTOR('',#17637,1.);
#5149=VECTOR('',#17638,1.);
#5150=VECTOR('',#17641,1.);
#5151=VECTOR('',#17642,1.);
#5152=VECTOR('',#17643,1.);
#5153=VECTOR('',#17646,1.);
#5154=VECTOR('',#17647,1.);
#5155=VECTOR('',#17648,1.);
#5156=VECTOR('',#17651,1.);
#5157=VECTOR('',#17652,1.);
#5158=VECTOR('',#17653,1.);
#5159=VECTOR('',#17656,1.);
#5160=VECTOR('',#17657,1.);
#5161=VECTOR('',#17658,1.);
#5162=VECTOR('',#17661,1.);
#5163=VECTOR('',#17662,1.);
#5164=VECTOR('',#17663,1.);
#5165=VECTOR('',#17666,1.);
#5166=VECTOR('',#17667,1.);
#5167=VECTOR('',#17668,1.);
#5168=VECTOR('',#17671,1.);
#5169=VECTOR('',#17672,1.);
#5170=VECTOR('',#17673,1.);
#5171=VECTOR('',#17676,1.);
#5172=VECTOR('',#17677,1.);
#5173=VECTOR('',#17678,1.);
#5174=VECTOR('',#17681,1.);
#5175=VECTOR('',#17682,1.);
#5176=VECTOR('',#17683,1.);
#5177=VECTOR('',#17686,1.);
#5178=VECTOR('',#17687,1.);
#5179=VECTOR('',#17688,1.);
#5180=VECTOR('',#17691,1.);
#5181=VECTOR('',#17692,1.);
#5182=VECTOR('',#17693,1.);
#5183=VECTOR('',#17696,1.);
#5184=VECTOR('',#17697,1.);
#5185=VECTOR('',#17698,1.);
#5186=VECTOR('',#17701,1.);
#5187=VECTOR('',#17702,1.);
#5188=VECTOR('',#17703,1.);
#5189=VECTOR('',#17706,1.);
#5190=VECTOR('',#17707,1.);
#5191=VECTOR('',#17708,1.);
#5192=VECTOR('',#17711,1.);
#5193=VECTOR('',#17712,1.);
#5194=VECTOR('',#17713,1.);
#5195=VECTOR('',#17716,1.);
#5196=VECTOR('',#17717,1.);
#5197=VECTOR('',#17718,1.);
#5198=VECTOR('',#17721,1.);
#5199=VECTOR('',#17722,1.);
#5200=VECTOR('',#17723,1.);
#5201=VECTOR('',#17726,1.);
#5202=VECTOR('',#17727,1.);
#5203=VECTOR('',#17728,1.);
#5204=VECTOR('',#17731,1.);
#5205=VECTOR('',#17732,1.);
#5206=VECTOR('',#17733,1.);
#5207=VECTOR('',#17736,1.);
#5208=VECTOR('',#17737,1.);
#5209=VECTOR('',#17738,1.);
#5210=VECTOR('',#17741,1.);
#5211=VECTOR('',#17742,1.);
#5212=VECTOR('',#17743,1.);
#5213=VECTOR('',#17746,1.);
#5214=VECTOR('',#17747,1.);
#5215=VECTOR('',#17748,1.);
#5216=VECTOR('',#17751,1.);
#5217=VECTOR('',#17752,1.);
#5218=VECTOR('',#17753,1.);
#5219=VECTOR('',#17756,1.);
#5220=VECTOR('',#17757,1.);
#5221=VECTOR('',#17758,1.);
#5222=VECTOR('',#17761,1.);
#5223=VECTOR('',#17762,1.);
#5224=VECTOR('',#17763,1.);
#5225=VECTOR('',#17766,1.);
#5226=VECTOR('',#17767,1.);
#5227=VECTOR('',#17768,1.);
#5228=VECTOR('',#17771,1.);
#5229=VECTOR('',#17772,1.);
#5230=VECTOR('',#17773,1.);
#5231=VECTOR('',#17776,1.);
#5232=VECTOR('',#17777,1.);
#5233=VECTOR('',#17778,1.);
#5234=VECTOR('',#17781,1.);
#5235=VECTOR('',#17782,1.);
#5236=VECTOR('',#17783,1.);
#5237=VECTOR('',#17786,1.);
#5238=VECTOR('',#17787,1.);
#5239=VECTOR('',#17788,1.);
#5240=VECTOR('',#17791,1.);
#5241=VECTOR('',#17792,1.);
#5242=VECTOR('',#17793,1.);
#5243=VECTOR('',#17796,1.);
#5244=VECTOR('',#17797,1.);
#5245=VECTOR('',#17798,1.);
#5246=VECTOR('',#17801,1.);
#5247=VECTOR('',#17802,1.);
#5248=VECTOR('',#17803,1.);
#5249=VECTOR('',#17806,1.);
#5250=VECTOR('',#17807,1.);
#5251=VECTOR('',#17808,1.);
#5252=VECTOR('',#17811,1.);
#5253=VECTOR('',#17812,1.);
#5254=VECTOR('',#17813,1.);
#5255=VECTOR('',#17816,1.);
#5256=VECTOR('',#17817,1.);
#5257=VECTOR('',#17818,1.);
#5258=VECTOR('',#17821,1.);
#5259=VECTOR('',#17822,1.);
#5260=VECTOR('',#17823,1.);
#5261=VECTOR('',#17826,1.);
#5262=VECTOR('',#17827,1.);
#5263=VECTOR('',#17828,1.);
#5264=VECTOR('',#17831,1.);
#5265=VECTOR('',#17832,1.);
#5266=VECTOR('',#17833,1.);
#5267=VECTOR('',#17836,1.);
#5268=VECTOR('',#17837,1.);
#5269=VECTOR('',#17838,1.);
#5270=VECTOR('',#17841,1.);
#5271=VECTOR('',#17842,1.);
#5272=VECTOR('',#17843,1.);
#5273=VECTOR('',#17846,1.);
#5274=VECTOR('',#17847,1.);
#5275=VECTOR('',#17848,1.);
#5276=VECTOR('',#17851,1.);
#5277=VECTOR('',#17852,1.);
#5278=VECTOR('',#17853,1.);
#5279=VECTOR('',#17856,1.);
#5280=VECTOR('',#17857,1.);
#5281=VECTOR('',#17858,1.);
#5282=VECTOR('',#17861,1.);
#5283=VECTOR('',#17862,1.);
#5284=VECTOR('',#17863,1.);
#5285=VECTOR('',#17866,1.);
#5286=VECTOR('',#17867,1.);
#5287=VECTOR('',#17868,1.);
#5288=VECTOR('',#17871,1.);
#5289=VECTOR('',#17872,1.);
#5290=VECTOR('',#17873,1.);
#5291=VECTOR('',#17876,1.);
#5292=VECTOR('',#17877,1.);
#5293=VECTOR('',#17878,1.);
#5294=VECTOR('',#17881,1.);
#5295=VECTOR('',#17882,1.);
#5296=VECTOR('',#17883,1.);
#5297=VECTOR('',#17886,1.);
#5298=VECTOR('',#17887,1.);
#5299=VECTOR('',#17888,1.);
#5300=VECTOR('',#17891,1.);
#5301=VECTOR('',#17892,1.);
#5302=VECTOR('',#17893,1.);
#5303=VECTOR('',#17896,1.);
#5304=VECTOR('',#17897,1.);
#5305=VECTOR('',#17898,1.);
#5306=VECTOR('',#17901,1.);
#5307=VECTOR('',#17902,1.);
#5308=VECTOR('',#17903,1.);
#5309=VECTOR('',#17906,1.);
#5310=VECTOR('',#17907,1.);
#5311=VECTOR('',#17908,1.);
#5312=VECTOR('',#17911,1.);
#5313=VECTOR('',#17912,1.);
#5314=VECTOR('',#17913,1.);
#5315=VECTOR('',#17916,1.);
#5316=VECTOR('',#17917,1.);
#5317=VECTOR('',#17918,1.);
#5318=VECTOR('',#17921,1.);
#5319=VECTOR('',#17922,1.);
#5320=VECTOR('',#17923,1.);
#5321=VECTOR('',#17926,1.);
#5322=VECTOR('',#17927,1.);
#5323=VECTOR('',#17928,1.);
#5324=VECTOR('',#17931,1.);
#5325=VECTOR('',#17932,1.);
#5326=VECTOR('',#17933,1.);
#5327=VECTOR('',#17936,1.);
#5328=VECTOR('',#17937,1.);
#5329=VECTOR('',#17938,1.);
#5330=VECTOR('',#17941,1.);
#5331=VECTOR('',#17942,1.);
#5332=VECTOR('',#17943,1.);
#5333=VECTOR('',#17946,1.);
#5334=VECTOR('',#17947,1.);
#5335=VECTOR('',#17948,1.);
#5336=VECTOR('',#17951,1.);
#5337=VECTOR('',#17952,1.);
#5338=VECTOR('',#17953,1.);
#5339=VECTOR('',#17956,1.);
#5340=VECTOR('',#17957,1.);
#5341=VECTOR('',#17958,1.);
#5342=VECTOR('',#17961,1.);
#5343=VECTOR('',#17962,1.);
#5344=VECTOR('',#17963,1.);
#5345=VECTOR('',#17966,1.);
#5346=VECTOR('',#17967,1.);
#5347=VECTOR('',#17968,1.);
#5348=VECTOR('',#17971,1.);
#5349=VECTOR('',#17972,1.);
#5350=VECTOR('',#17973,1.);
#5351=VECTOR('',#17976,1.);
#5352=VECTOR('',#17977,1.);
#5353=VECTOR('',#17978,1.);
#5354=VECTOR('',#17981,1.);
#5355=VECTOR('',#17982,1.);
#5356=VECTOR('',#17983,1.);
#5357=VECTOR('',#17986,1.);
#5358=VECTOR('',#17987,1.);
#5359=VECTOR('',#17988,1.);
#5360=VECTOR('',#17991,1.);
#5361=VECTOR('',#17992,1.);
#5362=VECTOR('',#17993,1.);
#5363=VECTOR('',#17996,1.);
#5364=VECTOR('',#17997,1.);
#5365=VECTOR('',#17998,1.);
#5366=VECTOR('',#18001,1.);
#5367=VECTOR('',#18002,1.);
#5368=VECTOR('',#18003,1.);
#5369=VECTOR('',#18006,1.);
#5370=VECTOR('',#18007,1.);
#5371=VECTOR('',#18008,1.);
#5372=VECTOR('',#18011,1.);
#5373=VECTOR('',#18012,1.);
#5374=VECTOR('',#18013,1.);
#5375=VECTOR('',#18016,1.);
#5376=VECTOR('',#18017,1.);
#5377=VECTOR('',#18018,1.);
#5378=VECTOR('',#18021,1.);
#5379=VECTOR('',#18022,1.);
#5380=VECTOR('',#18023,1.);
#5381=VECTOR('',#18026,1.);
#5382=VECTOR('',#18027,1.);
#5383=VECTOR('',#18028,1.);
#5384=VECTOR('',#18031,1.);
#5385=VECTOR('',#18032,1.);
#5386=VECTOR('',#18033,1.);
#5387=VECTOR('',#18036,1.);
#5388=VECTOR('',#18037,1.);
#5389=VECTOR('',#18038,1.);
#5390=VECTOR('',#18041,1.);
#5391=VECTOR('',#18042,1.);
#5392=VECTOR('',#18043,1.);
#5393=VECTOR('',#18046,1.);
#5394=VECTOR('',#18047,1.);
#5395=VECTOR('',#18048,1.);
#5396=VECTOR('',#18051,1.);
#5397=VECTOR('',#18052,1.);
#5398=VECTOR('',#18053,1.);
#5399=VECTOR('',#18056,1.);
#5400=VECTOR('',#18057,1.);
#5401=VECTOR('',#18058,1.);
#5402=VECTOR('',#18061,1.);
#5403=VECTOR('',#18062,1.);
#5404=VECTOR('',#18063,1.);
#5405=VECTOR('',#18066,1.);
#5406=VECTOR('',#18067,1.);
#5407=VECTOR('',#18068,1.);
#5408=VECTOR('',#18071,1.);
#5409=VECTOR('',#18072,1.);
#5410=VECTOR('',#18073,1.);
#5411=VECTOR('',#18076,1.);
#5412=VECTOR('',#18077,1.);
#5413=VECTOR('',#18088,1.);
#5414=VECTOR('',#18093,1.);
#5415=VECTOR('',#18096,0.21);
#5416=VECTOR('',#18101,1.);
#5417=VECTOR('',#18104,1.);
#5418=VECTOR('',#18109,1.);
#5419=VECTOR('',#18112,0.21);
#5420=VECTOR('',#18117,1.);
#5421=VECTOR('',#18120,1.);
#5422=VECTOR('',#18125,1.);
#5423=VECTOR('',#18128,0.21);
#5424=VECTOR('',#18133,1.);
#5425=VECTOR('',#18136,1.);
#5426=VECTOR('',#18141,1.);
#5427=VECTOR('',#18144,0.21);
#5428=VECTOR('',#18149,1.);
#5429=VECTOR('',#18152,1.);
#5430=VECTOR('',#18153,1.);
#5431=VECTOR('',#18154,1.);
#5432=VECTOR('',#18155,1.);
#5433=VECTOR('',#18156,1.);
#5434=VECTOR('',#18157,1.);
#5435=VECTOR('',#18160,1.);
#5436=VECTOR('',#18161,1.);
#5437=VECTOR('',#18162,1.);
#5438=VECTOR('',#18163,1.);
#5439=VECTOR('',#18164,1.);
#5440=VECTOR('',#18165,1.);
#5441=VECTOR('',#18168,1.);
#5442=VECTOR('',#18169,1.);
#5443=VECTOR('',#18170,1.);
#5444=VECTOR('',#18171,1.);
#5445=VECTOR('',#18172,1.);
#5446=VECTOR('',#18173,1.);
#5447=VECTOR('',#18174,1.);
#5448=VECTOR('',#18175,1.);
#5449=VECTOR('',#18176,1.);
#5450=VECTOR('',#18177,1.);
#5451=VECTOR('',#18180,1.);
#5452=VECTOR('',#18181,1.);
#5453=VECTOR('',#18184,1.);
#5454=VECTOR('',#18185,1.);
#5455=VECTOR('',#18188,1.);
#5456=VECTOR('',#18189,1.);
#5457=VECTOR('',#18192,1.);
#5458=VECTOR('',#18193,1.);
#5459=VECTOR('',#18196,1.);
#5460=VECTOR('',#18199,1.);
#5461=VECTOR('',#18200,1.);
#5462=VECTOR('',#18203,1.);
#5463=VECTOR('',#18204,1.);
#5464=VECTOR('',#18207,1.);
#5465=VECTOR('',#18208,1.);
#5466=VECTOR('',#18211,1.);
#5467=VECTOR('',#18212,1.);
#5468=VECTOR('',#18215,1.);
#5469=VECTOR('',#18222,1.);
#5470=VECTOR('',#18223,1.);
#5471=VECTOR('',#18224,1.);
#5472=VECTOR('',#18225,1.);
#5473=VECTOR('',#18228,1.);
#5474=VECTOR('',#18229,1.);
#5475=VECTOR('',#18230,1.);
#5476=VECTOR('',#18233,1.);
#5477=VECTOR('',#18234,1.);
#5478=VECTOR('',#18235,1.);
#5479=VECTOR('',#18238,1.);
#5480=VECTOR('',#18239,1.);
#5481=VECTOR('',#18240,1.);
#5482=VECTOR('',#18243,1.);
#5483=VECTOR('',#18244,1.);
#5484=VECTOR('',#18245,1.);
#5485=VECTOR('',#18248,1.);
#5486=VECTOR('',#18249,1.);
#5487=VECTOR('',#18250,1.);
#5488=VECTOR('',#18253,1.);
#5489=VECTOR('',#18254,1.);
#5490=VECTOR('',#18255,1.);
#5491=VECTOR('',#18258,1.);
#5492=VECTOR('',#18259,1.);
#5493=VECTOR('',#18268,1.);
#5494=VECTOR('',#18269,1.);
#5495=VECTOR('',#18270,1.);
#5496=VECTOR('',#18271,1.);
#5497=VECTOR('',#18274,1.);
#5498=VECTOR('',#18275,1.);
#5499=VECTOR('',#18276,1.);
#5500=VECTOR('',#18279,1.);
#5501=VECTOR('',#18280,1.);
#5502=VECTOR('',#18281,1.);
#5503=VECTOR('',#18284,1.);
#5504=VECTOR('',#18285,1.);
#5505=VECTOR('',#18286,1.);
#5506=VECTOR('',#18289,1.);
#5507=VECTOR('',#18290,1.);
#5508=VECTOR('',#18291,1.);
#5509=VECTOR('',#18294,1.);
#5510=VECTOR('',#18295,1.);
#5511=VECTOR('',#18296,1.);
#5512=VECTOR('',#18299,1.);
#5513=VECTOR('',#18300,1.);
#5514=VECTOR('',#18301,1.);
#5515=VECTOR('',#18304,1.);
#5516=VECTOR('',#18305,1.);
#5517=VECTOR('',#18320,1.);
#5518=VECTOR('',#18321,1.);
#5519=VECTOR('',#18322,1.);
#5520=VECTOR('',#18323,1.);
#5521=VECTOR('',#18326,1.);
#5522=VECTOR('',#18327,1.);
#5523=VECTOR('',#18328,1.);
#5524=VECTOR('',#18331,1.);
#5525=VECTOR('',#18332,1.);
#5526=VECTOR('',#18333,1.);
#5527=VECTOR('',#18336,1.);
#5528=VECTOR('',#18337,1.);
#5529=VECTOR('',#18338,1.);
#5530=VECTOR('',#18341,1.);
#5531=VECTOR('',#18342,1.);
#5532=VECTOR('',#18343,1.);
#5533=VECTOR('',#18346,1.);
#5534=VECTOR('',#18347,1.);
#5535=VECTOR('',#18364,0.4);
#5536=VECTOR('',#18369,0.425);
#5537=VECTOR('',#18374,0.41);
#5538=VECTOR('',#18383,0.26);
#5539=VECTOR('',#18386,0.25);
#5540=VECTOR('',#18393,1.);
#5541=VECTOR('',#18394,1.);
#5542=VECTOR('',#18395,1.);
#5543=VECTOR('',#18396,1.);
#5544=VECTOR('',#18401,1.);
#5545=VECTOR('',#18402,1.);
#5546=VECTOR('',#18405,1.);
#5547=VECTOR('',#18406,1.);
#5548=VECTOR('',#18407,1.);
#5549=VECTOR('',#18410,1.);
#5550=VECTOR('',#18419,0.164999999999999);
#5551=VECTOR('',#18428,0.164999999999999);
#5552=VECTOR('',#18435,1.);
#5553=VECTOR('',#18436,1.);
#5554=VECTOR('',#18437,1.);
#5555=VECTOR('',#18438,1.);
#5556=VECTOR('',#18443,1.);
#5557=VECTOR('',#18444,1.);
#5558=VECTOR('',#18447,1.);
#5559=VECTOR('',#18448,1.);
#5560=VECTOR('',#18449,1.);
#5561=VECTOR('',#18452,1.);
#5562=VECTOR('',#18471,0.800000000000001);
#5563=VECTOR('',#18474,0.6);
#5564=VECTOR('',#18481,0.6);
#5565=VECTOR('',#18492,0.605);
#5566=VECTOR('',#18499,0.800000000000001);
#5567=VECTOR('',#18512,0.605);
#5568=VECTOR('',#18519,0.800000000000001);
#5569=VECTOR('',#18532,0.605);
#5570=VECTOR('',#18539,0.800000000000001);
#5571=VECTOR('',#18552,0.225);
#5572=VECTOR('',#18559,1.);
#5573=VECTOR('',#18572,0.225);
#5574=VECTOR('',#18579,1.);
#5575=VECTOR('',#18592,0.605);
#5576=VECTOR('',#18599,0.800000000000001);
#5577=VECTOR('',#18612,0.25);
#5578=VECTOR('',#18617,1.);
#5579=VECTOR('',#18618,1.);
#5580=VECTOR('',#18619,1.);
#5581=VECTOR('',#18620,1.);
#5582=VECTOR('',#18623,1.);
#5583=VECTOR('',#18624,1.);
#5584=VECTOR('',#18625,1.);
#5585=VECTOR('',#18628,1.);
#5586=VECTOR('',#18629,1.);
#5587=VECTOR('',#18630,1.);
#5588=VECTOR('',#18643,1.);
#5589=VECTOR('',#18646,1.);
#5590=VECTOR('',#18651,1.);
#5591=VECTOR('',#18652,1.);
#5592=VECTOR('',#18653,1.);
#5593=VECTOR('',#18656,1.);
#5594=VECTOR('',#18661,1.);
#5595=VECTOR('',#18662,1.);
#5596=VECTOR('',#18669,1.2);
#5597=VECTOR('',#18680,0.33);
#5598=VECTOR('',#18687,0.4);
#5599=VECTOR('',#18698,1.);
#5600=VECTOR('',#18699,1.);
#5601=VECTOR('',#18700,1.);
#5602=VECTOR('',#18701,1.);
#5603=VECTOR('',#18704,1.);
#5604=VECTOR('',#18705,1.);
#5605=VECTOR('',#18706,1.);
#5606=VECTOR('',#18709,1.);
#5607=VECTOR('',#18710,1.);
#5608=VECTOR('',#18711,1.);
#5609=VECTOR('',#18716,1.);
#5610=VECTOR('',#18719,1.);
#5611=VECTOR('',#18722,1.);
#5612=VECTOR('',#18725,1.);
#5613=VECTOR('',#18728,1.);
#5614=VECTOR('',#18731,1.);
#5615=VECTOR('',#18734,1.);
#5616=VECTOR('',#18737,1.);
#5617=VECTOR('',#18740,1.);
#5618=VECTOR('',#18743,1.);
#5619=VECTOR('',#18746,1.);
#5620=VECTOR('',#18749,1.);
#5621=VECTOR('',#18752,1.);
#5622=VECTOR('',#18755,1.);
#5623=VECTOR('',#18758,1.);
#5624=VECTOR('',#18761,1.);
#5625=VECTOR('',#18764,1.);
#5626=VECTOR('',#18767,1.);
#5627=VECTOR('',#18770,1.);
#5628=VECTOR('',#18773,1.);
#5629=VECTOR('',#18784,1.4);
#5630=VECTOR('',#18789,1.);
#5631=VECTOR('',#18790,1.);
#5632=VECTOR('',#18793,1.);
#5633=VECTOR('',#18794,1.);
#5634=VECTOR('',#18795,1.);
#5635=VECTOR('',#18800,1.);
#5636=VECTOR('',#18801,1.);
#5637=VECTOR('',#18804,1.);
#5638=VECTOR('',#18805,1.);
#5639=VECTOR('',#18806,1.);
#5640=VECTOR('',#18811,1.);
#5641=VECTOR('',#18812,1.);
#5642=VECTOR('',#18815,1.);
#5643=VECTOR('',#18816,1.);
#5644=VECTOR('',#18817,1.);
#5645=VECTOR('',#18822,1.);
#5646=VECTOR('',#18823,1.);
#5647=VECTOR('',#18826,1.);
#5648=VECTOR('',#18827,1.);
#5649=VECTOR('',#18828,1.);
#5650=VECTOR('',#18833,1.);
#5651=VECTOR('',#18834,1.);
#5652=VECTOR('',#18837,1.);
#5653=VECTOR('',#18838,1.);
#5654=VECTOR('',#18839,1.);
#5655=VECTOR('',#18844,1.);
#5656=VECTOR('',#18845,1.);
#5657=VECTOR('',#18848,1.);
#5658=VECTOR('',#18849,1.);
#5659=VECTOR('',#18850,1.);
#5660=VECTOR('',#18855,1.);
#5661=VECTOR('',#18856,1.);
#5662=VECTOR('',#18859,1.);
#5663=VECTOR('',#18860,1.);
#5664=VECTOR('',#18861,1.);
#5665=VECTOR('',#18866,1.);
#5666=VECTOR('',#18867,1.);
#5667=VECTOR('',#18870,1.);
#5668=VECTOR('',#18871,1.);
#5669=VECTOR('',#18872,1.);
#5670=VECTOR('',#18877,1.);
#5671=VECTOR('',#18878,1.);
#5672=VECTOR('',#18881,1.);
#5673=VECTOR('',#18882,1.);
#5674=VECTOR('',#18883,1.);
#5675=VECTOR('',#18888,1.);
#5676=VECTOR('',#18889,1.);
#5677=VECTOR('',#18892,1.);
#5678=VECTOR('',#18893,1.);
#5679=VECTOR('',#18894,1.);
#5680=VECTOR('',#18899,1.);
#5681=VECTOR('',#18900,1.);
#5682=VECTOR('',#18903,1.);
#5683=VECTOR('',#18904,1.);
#5684=VECTOR('',#18905,1.);
#5685=VECTOR('',#18910,1.);
#5686=VECTOR('',#18911,1.);
#5687=VECTOR('',#18914,1.);
#5688=VECTOR('',#18915,1.);
#5689=VECTOR('',#18916,1.);
#5690=VECTOR('',#18921,1.);
#5691=VECTOR('',#18922,1.);
#5692=VECTOR('',#18925,1.);
#5693=VECTOR('',#18926,1.);
#5694=VECTOR('',#18927,1.);
#5695=VECTOR('',#18932,1.);
#5696=VECTOR('',#18933,1.);
#5697=VECTOR('',#18936,1.);
#5698=VECTOR('',#18937,1.);
#5699=VECTOR('',#18938,1.);
#5700=VECTOR('',#18943,1.);
#5701=VECTOR('',#18944,1.);
#5702=VECTOR('',#18947,1.);
#5703=VECTOR('',#18948,1.);
#5704=VECTOR('',#18949,1.);
#5705=VECTOR('',#18954,1.);
#5706=VECTOR('',#18955,1.);
#5707=VECTOR('',#18958,1.);
#5708=VECTOR('',#18959,1.);
#5709=VECTOR('',#18960,1.);
#5710=VECTOR('',#18965,1.);
#5711=VECTOR('',#18966,1.);
#5712=VECTOR('',#18969,1.);
#5713=VECTOR('',#18970,1.);
#5714=VECTOR('',#18971,1.);
#5715=VECTOR('',#18976,1.);
#5716=VECTOR('',#18977,1.);
#5717=VECTOR('',#18980,1.);
#5718=VECTOR('',#18981,1.);
#5719=VECTOR('',#18982,1.);
#5720=VECTOR('',#18987,1.);
#5721=VECTOR('',#18988,1.);
#5722=VECTOR('',#18991,1.);
#5723=VECTOR('',#18992,1.);
#5724=VECTOR('',#18993,1.);
#5725=VECTOR('',#18998,1.);
#5726=VECTOR('',#18999,1.);
#5727=VECTOR('',#19002,1.);
#5728=VECTOR('',#19003,1.);
#5729=VECTOR('',#19004,1.);
#5730=VECTOR('',#19021,0.325);
#5731=VECTOR('',#19026,0.35);
#5732=VECTOR('',#19031,0.335);
#5733=VECTOR('',#19040,0.21);
#5734=VECTOR('',#19045,0.2);
#5735=VECTOR('',#19050,0.18);
#5736=VECTOR('',#19055,1.);
#5737=VECTOR('',#19056,1.);
#5738=VECTOR('',#19057,1.);
#5739=VECTOR('',#19058,1.);
#5740=VECTOR('',#19061,1.);
#5741=VECTOR('',#19062,1.);
#5742=VECTOR('',#19063,1.);
#5743=VECTOR('',#19066,1.);
#5744=VECTOR('',#19067,1.);
#5745=VECTOR('',#19068,1.);
#5746=VECTOR('',#19071,1.);
#5747=VECTOR('',#19072,1.);
#5748=VECTOR('',#19073,1.);
#5749=VECTOR('',#19076,1.);
#5750=VECTOR('',#19077,1.);
#5751=VECTOR('',#19078,1.);
#5752=VECTOR('',#19081,1.);
#5753=VECTOR('',#19082,1.);
#5754=VECTOR('',#19255,1.);
#5755=VECTOR('',#19256,1.);
#5756=VECTOR('',#19257,1.);
#5757=VECTOR('',#19258,1.);
#5758=VECTOR('',#19259,1.);
#5759=VECTOR('',#19260,1.);
#5760=VECTOR('',#19261,1.);
#5761=VECTOR('',#19262,1.);
#5762=VECTOR('',#19265,1.);
#5763=VECTOR('',#19266,1.);
#5764=VECTOR('',#19267,1.);
#5765=VECTOR('',#19270,1.);
#5766=VECTOR('',#19271,1.);
#5767=VECTOR('',#19274,1.);
#5768=VECTOR('',#19275,1.);
#5769=VECTOR('',#19278,1.);
#5770=VECTOR('',#19279,1.);
#5771=VECTOR('',#19282,1.);
#5772=VECTOR('',#19283,1.);
#5773=VECTOR('',#19284,1.);
#5774=VECTOR('',#19285,1.);
#5775=VECTOR('',#19288,1.);
#5776=VECTOR('',#19291,1.);
#5777=VECTOR('',#19294,1.);
#5778=VECTOR('',#19303,0.32);
#5779=VECTOR('',#19310,0.6);
#5780=VECTOR('',#19327,0.475);
#5781=VECTOR('',#19332,0.5);
#5782=VECTOR('',#19337,0.485);
#5783=VECTOR('',#19346,0.31);
#5784=VECTOR('',#19351,0.3);
#5785=VECTOR('',#19356,0.27);
#5786=VECTOR('',#19361,1.);
#5787=VECTOR('',#19362,1.);
#5788=VECTOR('',#19363,1.);
#5789=VECTOR('',#19364,1.);
#5790=VECTOR('',#19367,1.);
#5791=VECTOR('',#19368,1.);
#5792=VECTOR('',#19369,1.);
#5793=VECTOR('',#19372,1.);
#5794=VECTOR('',#19373,1.);
#5795=VECTOR('',#19374,1.);
#5796=VECTOR('',#19377,1.);
#5797=VECTOR('',#19378,1.);
#5798=VECTOR('',#19379,1.);
#5799=VECTOR('',#19382,1.);
#5800=VECTOR('',#19383,1.);
#5801=VECTOR('',#19384,1.);
#5802=VECTOR('',#19387,1.);
#5803=VECTOR('',#19388,1.);
#5804=VECTOR('',#19433,0.404999999999999);
#5805=VECTOR('',#19440,0.9);
#5806=CIRCLE('',#14321,0.274999999999999);
#5807=CIRCLE('',#14322,0.274999999999999);
#5808=CIRCLE('',#14324,0.274999999999999);
#5809=CIRCLE('',#14325,0.274999999999999);
#5810=CIRCLE('',#14327,0.275);
#5811=CIRCLE('',#14328,0.275);
#5812=CIRCLE('',#14330,0.275);
#5813=CIRCLE('',#14331,0.275);
#5814=CIRCLE('',#14354,0.164999999999999);
#5815=CIRCLE('',#14355,0.164999999999999);
#5816=CIRCLE('',#14357,0.164999999999999);
#5817=CIRCLE('',#14358,0.164999999999999);
#5818=CIRCLE('',#14360,0.164999999999999);
#5819=CIRCLE('',#14361,0.164999999999999);
#5820=CIRCLE('',#14363,0.164999999999999);
#5821=CIRCLE('',#14364,0.164999999999999);
#5822=CIRCLE('',#14366,0.210000000000001);
#5823=CIRCLE('',#14367,0.210000000000001);
#5824=CIRCLE('',#14369,0.210000000000001);
#5825=CIRCLE('',#14370,0.210000000000001);
#5826=CIRCLE('',#14372,0.21);
#5827=CIRCLE('',#14373,0.21);
#5828=CIRCLE('',#14375,0.21);
#5829=CIRCLE('',#14376,0.21);
#5830=CIRCLE('',#14378,0.164999999999999);
#5831=CIRCLE('',#14379,0.164999999999999);
#5832=CIRCLE('',#14381,0.164999999999999);
#5833=CIRCLE('',#14382,0.164999999999999);
#5834=CIRCLE('',#14384,0.165);
#5835=CIRCLE('',#14385,0.165);
#5836=CIRCLE('',#14387,0.164999999999999);
#5837=CIRCLE('',#14388,0.164999999999999);
#5838=CIRCLE('',#14390,0.274999999999999);
#5839=CIRCLE('',#14391,0.274999999999999);
#5840=CIRCLE('',#14393,0.274999999999999);
#5841=CIRCLE('',#14394,0.274999999999999);
#5842=CIRCLE('',#14396,0.275);
#5843=CIRCLE('',#14397,0.275);
#5844=CIRCLE('',#14399,0.275);
#5845=CIRCLE('',#14400,0.275);
#5846=CIRCLE('',#14409,0.5);
#5847=CIRCLE('',#14410,0.5);
#5848=CIRCLE('',#14412,0.275);
#5849=CIRCLE('',#14414,0.5);
#5850=CIRCLE('',#14415,0.5);
#5851=CIRCLE('',#14417,0.275);
#5852=CIRCLE('',#14419,0.275);
#5853=CIRCLE('',#14421,0.275);
#5854=CIRCLE('',#14437,0.5);
#5855=CIRCLE('',#14438,0.5);
#5856=CIRCLE('',#14440,0.274999999999999);
#5857=CIRCLE('',#14442,0.5);
#5858=CIRCLE('',#14443,0.5);
#5859=CIRCLE('',#14445,0.274999999999999);
#5860=CIRCLE('',#14447,0.274999999999999);
#5861=CIRCLE('',#14449,0.274999999999999);
#5862=CIRCLE('',#14465,0.225);
#5863=CIRCLE('',#14466,0.225);
#5864=CIRCLE('',#14468,0.225);
#5865=CIRCLE('',#14469,0.225);
#5866=CIRCLE('',#14471,0.164999999999999);
#5867=CIRCLE('',#14472,0.164999999999999);
#5868=CIRCLE('',#14474,0.164999999999999);
#5869=CIRCLE('',#14475,0.164999999999999);
#5870=CIRCLE('',#14477,0.164999999999999);
#5871=CIRCLE('',#14478,0.164999999999999);
#5872=CIRCLE('',#14480,0.164999999999999);
#5873=CIRCLE('',#14481,0.164999999999999);
#5874=CIRCLE('',#14483,1.6);
#5875=CIRCLE('',#14484,1.6);
#5876=CIRCLE('',#14497,0.225);
#5877=CIRCLE('',#14498,0.225);
#5878=CIRCLE('',#14500,0.225);
#5879=CIRCLE('',#14501,0.225);
#5880=CIRCLE('',#14503,0.225);
#5881=CIRCLE('',#14504,0.225);
#5882=CIRCLE('',#14506,0.225);
#5883=CIRCLE('',#14507,0.225);
#5884=CIRCLE('',#14509,1.59);
#5885=CIRCLE('',#14510,1.59);
#5886=CIRCLE('',#14512,1.2);
#5887=CIRCLE('',#14514,1.2);
#5888=CIRCLE('',#14516,2.4);
#5889=CIRCLE('',#14517,2.4);
#5890=CIRCLE('',#14522,0.225);
#5891=CIRCLE('',#14523,0.225);
#5892=CIRCLE('',#14525,0.225);
#5893=CIRCLE('',#14526,0.225);
#5894=CIRCLE('',#14528,0.225);
#5895=CIRCLE('',#14529,0.225);
#5896=CIRCLE('',#14531,0.225);
#5897=CIRCLE('',#14532,0.225);
#5898=CIRCLE('',#14534,1.59);
#5899=CIRCLE('',#14535,1.59);
#5900=CIRCLE('',#14537,1.2);
#5901=CIRCLE('',#14539,1.2);
#5902=CIRCLE('',#14541,2.4);
#5903=CIRCLE('',#14542,2.4);
#5904=CIRCLE('',#14547,0.225);
#5905=CIRCLE('',#14548,0.225);
#5906=CIRCLE('',#14550,0.225);
#5907=CIRCLE('',#14551,0.225);
#5908=CIRCLE('',#14553,0.164999999999999);
#5909=CIRCLE('',#14554,0.164999999999999);
#5910=CIRCLE('',#14556,0.164999999999999);
#5911=CIRCLE('',#14557,0.164999999999999);
#5912=CIRCLE('',#14559,0.164999999999999);
#5913=CIRCLE('',#14560,0.164999999999999);
#5914=CIRCLE('',#14562,0.164999999999999);
#5915=CIRCLE('',#14563,0.164999999999999);
#5916=CIRCLE('',#14565,1.6);
#5917=CIRCLE('',#14566,1.6);
#5918=CIRCLE('',#14579,0.225);
#5919=CIRCLE('',#14580,0.225);
#5920=CIRCLE('',#14582,0.225);
#5921=CIRCLE('',#14583,0.225);
#5922=CIRCLE('',#14585,0.225);
#5923=CIRCLE('',#14586,0.225);
#5924=CIRCLE('',#14588,0.225);
#5925=CIRCLE('',#14589,0.225);
#5926=CIRCLE('',#14591,1.59);
#5927=CIRCLE('',#14592,1.59);
#5928=CIRCLE('',#14594,1.2);
#5929=CIRCLE('',#14596,1.2);
#5930=CIRCLE('',#14598,2.4);
#5931=CIRCLE('',#14599,2.4);
#5932=CIRCLE('',#14604,0.225);
#5933=CIRCLE('',#14605,0.225);
#5934=CIRCLE('',#14607,0.225);
#5935=CIRCLE('',#14608,0.225);
#5936=CIRCLE('',#14610,0.225);
#5937=CIRCLE('',#14611,0.225);
#5938=CIRCLE('',#14613,0.225);
#5939=CIRCLE('',#14614,0.225);
#5940=CIRCLE('',#14616,1.59);
#5941=CIRCLE('',#14617,1.59);
#5942=CIRCLE('',#14619,1.2);
#5943=CIRCLE('',#14621,1.2);
#5944=CIRCLE('',#14623,2.4);
#5945=CIRCLE('',#14624,2.4);
#5946=CIRCLE('',#14665,0.21);
#5947=CIRCLE('',#14666,0.21);
#5948=CIRCLE('',#14681,0.2117);
#5949=CIRCLE('',#14690,0.2117);
#5950=CIRCLE('',#14691,0.2117);
#5951=CIRCLE('',#14693,0.2117);
#5952=CIRCLE('',#14700,0.285);
#5953=CIRCLE('',#14701,0.265);
#5954=CIRCLE('',#14703,0.265);
#5955=CIRCLE('',#14705,0.5);
#5956=CIRCLE('',#14707,0.5);
#5957=CIRCLE('',#14711,0.375);
#5958=CIRCLE('',#14712,0.375);
#5959=CIRCLE('',#14714,0.225);
#5960=CIRCLE('',#14716,0.375);
#5961=CIRCLE('',#14717,0.375);
#5962=CIRCLE('',#14719,0.225);
#5963=CIRCLE('',#14721,0.375);
#5964=CIRCLE('',#14722,0.375);
#5965=CIRCLE('',#14724,0.225);
#5966=CIRCLE('',#14726,0.375);
#5967=CIRCLE('',#14727,0.375);
#5968=CIRCLE('',#14729,0.225000000000001);
#5969=CIRCLE('',#14731,0.225);
#5970=CIRCLE('',#14733,0.225);
#5971=CIRCLE('',#14735,0.225);
#5972=CIRCLE('',#14737,0.225000000000001);
#5973=CIRCLE('',#14754,0.375);
#5974=CIRCLE('',#14756,0.425);
#5975=CIRCLE('',#14758,0.425);
#5976=CIRCLE('',#14760,0.395);
#5977=CIRCLE('',#14762,0.27);
#5978=CIRCLE('',#14764,0.24505);
#5979=CIRCLE('',#14766,0.24505);
#5980=CIRCLE('',#14768,0.2);
#5981=CIRCLE('',#14781,1.070235);
#5982=CIRCLE('',#14782,1.070235);
#5983=CIRCLE('',#14783,0.309556);
#5984=CIRCLE('',#14784,1.070235);
#5985=CIRCLE('',#14785,1.070235);
#5986=CIRCLE('',#14787,1.070235);
#5987=CIRCLE('',#14789,0.6);
#5988=CIRCLE('',#14790,0.6);
#5989=CIRCLE('',#14792,0.66);
#5990=CIRCLE('',#14795,1.070235);
#5991=CIRCLE('',#14797,0.66);
#5992=CIRCLE('',#14801,1.129765);
#5993=CIRCLE('',#14802,1.129765);
#5994=CIRCLE('',#14803,0.309556);
#5995=CIRCLE('',#14804,1.129765);
#5996=CIRCLE('',#14805,1.129765);
#5997=CIRCLE('',#14807,1.129765);
#5998=CIRCLE('',#14809,1.54);
#5999=CIRCLE('',#14810,1.129765);
#6000=CIRCLE('',#14812,1.6);
#6001=CIRCLE('',#14814,1.6);
#6002=CIRCLE('',#14816,1.54);
#6003=CIRCLE('',#14821,0.29765);
#6004=CIRCLE('',#14823,0.29765);
#6005=CIRCLE('',#14825,0.29765);
#6006=CIRCLE('',#14827,0.29765);
#6007=CIRCLE('',#14829,0.29765);
#6008=CIRCLE('',#14831,0.29765);
#6009=CIRCLE('',#14833,0.29765);
#6010=CIRCLE('',#14836,0.303778037777585);
#6011=CIRCLE('',#14837,0.303778037777585);
#6012=CIRCLE('',#14839,1.123812);
#6013=CIRCLE('',#14840,1.123812);
#6014=CIRCLE('',#14841,1.123812);
#6015=CIRCLE('',#14842,1.123812);
#6016=CIRCLE('',#14843,1.123812);
#6017=CIRCLE('',#14844,1.123812);
#6018=CIRCLE('',#14845,1.123812);
#6019=CIRCLE('',#14846,1.123812);
#6020=CIRCLE('',#14847,1.123812);
#6021=CIRCLE('',#14849,1.076188);
#6022=CIRCLE('',#14850,0.303778037777585);
#6023=CIRCLE('',#14852,0.303778037777585);
#6024=CIRCLE('',#14854,1.076188);
#6025=CIRCLE('',#14855,0.303778037777585);
#6026=CIRCLE('',#14857,0.303778037777585);
#6027=CIRCLE('',#14859,1.076188);
#6028=CIRCLE('',#14860,1.076188);
#6029=CIRCLE('',#14861,0.303778037777585);
#6030=CIRCLE('',#14863,0.303778037777585);
#6031=CIRCLE('',#14865,1.076188);
#6032=CIRCLE('',#14866,0.303778037777585);
#6033=CIRCLE('',#14868,0.303778037777585);
#6034=CIRCLE('',#14870,1.076188);
#6035=CIRCLE('',#14871,0.303778037777585);
#6036=CIRCLE('',#14873,0.303778037777585);
#6037=CIRCLE('',#14875,1.076188);
#6038=CIRCLE('',#14876,1.076188);
#6039=CIRCLE('',#14877,1.076188);
#6040=CIRCLE('',#14879,0.303778037777585);
#6041=CIRCLE('',#14881,0.303778037777585);
#6042=CIRCLE('',#14886,1.119765);
#6043=CIRCLE('',#14887,1.085235);
#6044=CIRCLE('',#14889,1.119765);
#6045=CIRCLE('',#14891,1.085235);
#6046=CIRCLE('',#14894,1.119765);
#6047=CIRCLE('',#14895,1.085235);
#6048=CIRCLE('',#14897,1.119765);
#6049=CIRCLE('',#14899,1.085235);
#6050=CIRCLE('',#14916,0.1954);
#6051=CIRCLE('',#14918,0.3);
#6052=CIRCLE('',#14920,0.35);
#6053=CIRCLE('',#14922,0.35);
#6054=CIRCLE('',#14924,0.32);
#6055=CIRCLE('',#14926,0.22);
#6056=CIRCLE('',#14928,0.1954);
#6057=CIRCLE('',#14933,0.225000000000001);
#6058=CIRCLE('',#14934,0.225000000000001);
#6059=CIRCLE('',#14936,0.225);
#6060=CIRCLE('',#14937,0.225);
#6061=CIRCLE('',#14939,0.225);
#6062=CIRCLE('',#14940,0.225);
#6063=CIRCLE('',#14942,0.225000000000001);
#6064=CIRCLE('',#14943,0.225000000000001);
#6065=CIRCLE('',#14945,0.275);
#6066=CIRCLE('',#14946,0.275);
#6067=CIRCLE('',#14948,0.275);
#6068=CIRCLE('',#14949,0.275);
#6069=CIRCLE('',#14951,0.275);
#6070=CIRCLE('',#14952,0.275);
#6071=CIRCLE('',#14954,0.275);
#6072=CIRCLE('',#14955,0.275);
#6073=CIRCLE('',#14964,0.164999999999999);
#6074=CIRCLE('',#14965,0.164999999999999);
#6075=CIRCLE('',#14968,0.165);
#6076=CIRCLE('',#14969,0.165);
#6077=CIRCLE('',#14972,0.165);
#6078=CIRCLE('',#14973,0.165);
#6079=CIRCLE('',#14976,0.164999999999999);
#6080=CIRCLE('',#14977,0.164999999999999);
#6081=CIRCLE('',#15112,0.21);
#6082=CIRCLE('',#15114,0.21);
#6083=CIRCLE('',#15115,0.21);
#6084=CIRCLE('',#15116,0.21);
#6085=CIRCLE('',#15118,0.21);
#6086=CIRCLE('',#15120,0.21);
#6087=CIRCLE('',#15121,0.21);
#6088=CIRCLE('',#15122,0.21);
#6089=CIRCLE('',#15124,0.21);
#6090=CIRCLE('',#15126,0.21);
#6091=CIRCLE('',#15127,0.21);
#6092=CIRCLE('',#15128,0.21);
#6093=CIRCLE('',#15130,0.21);
#6094=CIRCLE('',#15132,0.21);
#6095=CIRCLE('',#15133,0.21);
#6096=CIRCLE('',#15134,0.21);
#6097=CIRCLE('',#15184,0.24505);
#6098=CIRCLE('',#15186,0.375);
#6099=CIRCLE('',#15188,0.425);
#6100=CIRCLE('',#15190,0.425);
#6101=CIRCLE('',#15192,0.395);
#6102=CIRCLE('',#15194,0.27);
#6103=CIRCLE('',#15196,0.24505);
#6104=CIRCLE('',#15202,0.6);
#6105=CIRCLE('',#15206,0.6);
#6106=CIRCLE('',#15208,0.164999999999999);
#6107=CIRCLE('',#15209,0.164999999999999);
#6108=CIRCLE('',#15212,0.164999999999999);
#6109=CIRCLE('',#15213,0.164999999999999);
#6110=CIRCLE('',#15217,0.6);
#6111=CIRCLE('',#15221,0.6);
#6112=CIRCLE('',#15223,0.800000000000001);
#6113=CIRCLE('',#15224,0.6);
#6114=CIRCLE('',#15226,0.800000000000001);
#6115=CIRCLE('',#15227,0.6);
#6116=CIRCLE('',#15230,0.6);
#6117=CIRCLE('',#15232,0.6);
#6118=CIRCLE('',#15237,0.605);
#6119=CIRCLE('',#15238,0.605);
#6120=CIRCLE('',#15240,0.800000000000001);
#6121=CIRCLE('',#15241,0.800000000000001);
#6122=CIRCLE('',#15246,0.605);
#6123=CIRCLE('',#15247,0.605);
#6124=CIRCLE('',#15249,0.800000000000001);
#6125=CIRCLE('',#15250,0.800000000000001);
#6126=CIRCLE('',#15255,0.605);
#6127=CIRCLE('',#15256,0.605);
#6128=CIRCLE('',#15258,0.800000000000001);
#6129=CIRCLE('',#15259,0.800000000000001);
#6130=CIRCLE('',#15264,0.225);
#6131=CIRCLE('',#15265,0.225);
#6132=CIRCLE('',#15267,1.);
#6133=CIRCLE('',#15268,1.);
#6134=CIRCLE('',#15273,0.225);
#6135=CIRCLE('',#15274,0.225);
#6136=CIRCLE('',#15276,1.);
#6137=CIRCLE('',#15277,1.);
#6138=CIRCLE('',#15282,0.605);
#6139=CIRCLE('',#15283,0.605);
#6140=CIRCLE('',#15285,0.800000000000001);
#6141=CIRCLE('',#15286,0.800000000000001);
#6142=CIRCLE('',#15291,0.25);
#6143=CIRCLE('',#15292,0.25);
#6144=CIRCLE('',#15297,1.2);
#6145=CIRCLE('',#15298,0.6);
#6146=CIRCLE('',#15300,0.6);
#6147=CIRCLE('',#15302,0.9);
#6148=CIRCLE('',#15303,0.9);
#6149=CIRCLE('',#15306,1.2);
#6150=CIRCLE('',#15309,1.2);
#6151=CIRCLE('',#15311,1.2);
#6152=CIRCLE('',#15315,0.33);
#6153=CIRCLE('',#15316,0.33);
#6154=CIRCLE('',#15318,0.4);
#6155=CIRCLE('',#15319,0.4);
#6156=CIRCLE('',#15327,1.75);
#6157=CIRCLE('',#15328,1.75);
#6158=CIRCLE('',#15329,1.75);
#6159=CIRCLE('',#15330,1.75);
#6160=CIRCLE('',#15331,1.75);
#6161=CIRCLE('',#15332,1.75);
#6162=CIRCLE('',#15333,1.75);
#6163=CIRCLE('',#15334,1.75);
#6164=CIRCLE('',#15335,1.75);
#6165=CIRCLE('',#15336,1.75);
#6166=CIRCLE('',#15337,1.75);
#6167=CIRCLE('',#15338,1.75);
#6168=CIRCLE('',#15339,1.75);
#6169=CIRCLE('',#15340,1.75);
#6170=CIRCLE('',#15341,1.75);
#6171=CIRCLE('',#15342,1.75);
#6172=CIRCLE('',#15343,1.75);
#6173=CIRCLE('',#15344,1.75);
#6174=CIRCLE('',#15345,1.75);
#6175=CIRCLE('',#15346,1.75);
#6176=CIRCLE('',#15347,0.6);
#6177=CIRCLE('',#15349,0.6);
#6178=CIRCLE('',#15351,1.4);
#6179=CIRCLE('',#15352,1.4);
#6180=CIRCLE('',#15356,1.75);
#6181=CIRCLE('',#15359,1.75);
#6182=CIRCLE('',#15362,1.75);
#6183=CIRCLE('',#15365,1.75);
#6184=CIRCLE('',#15368,1.75);
#6185=CIRCLE('',#15371,1.75);
#6186=CIRCLE('',#15374,1.75);
#6187=CIRCLE('',#15377,1.75);
#6188=CIRCLE('',#15380,1.75);
#6189=CIRCLE('',#15383,1.75);
#6190=CIRCLE('',#15386,1.75);
#6191=CIRCLE('',#15389,1.75);
#6192=CIRCLE('',#15392,1.75);
#6193=CIRCLE('',#15395,1.75);
#6194=CIRCLE('',#15398,1.75);
#6195=CIRCLE('',#15401,1.75);
#6196=CIRCLE('',#15404,1.75);
#6197=CIRCLE('',#15407,1.75);
#6198=CIRCLE('',#15410,1.75);
#6199=CIRCLE('',#15413,1.75);
#6200=CIRCLE('',#15417,0.3);
#6201=CIRCLE('',#15419,0.35);
#6202=CIRCLE('',#15421,0.35);
#6203=CIRCLE('',#15423,0.32);
#6204=CIRCLE('',#15425,0.22);
#6205=CIRCLE('',#15427,0.1954);
#6206=CIRCLE('',#15429,0.1954);
#6207=CIRCLE('',#15431,0.16);
#6208=CIRCLE('',#15536,0.32);
#6209=CIRCLE('',#15537,0.32);
#6210=CIRCLE('',#15539,0.6);
#6211=CIRCLE('',#15540,0.6);
#6212=CIRCLE('',#15545,0.45);
#6213=CIRCLE('',#15547,0.5);
#6214=CIRCLE('',#15549,0.5);
#6215=CIRCLE('',#15551,0.47);
#6216=CIRCLE('',#15553,0.32);
#6217=CIRCLE('',#15555,0.2942);
#6218=CIRCLE('',#15557,0.2942);
#6219=CIRCLE('',#15559,0.24);
#6220=CIRCLE('',#15588,0.404999999999999);
#6221=CIRCLE('',#15589,0.404999999999999);
#6222=CIRCLE('',#15591,0.9);
#6223=CIRCLE('',#15592,0.9);
#6224=VERTEX_POINT('',#19461);
#6225=VERTEX_POINT('',#19463);
#6226=VERTEX_POINT('',#19467);
#6227=VERTEX_POINT('',#19469);
#6228=VERTEX_POINT('',#19473);
#6229=VERTEX_POINT('',#19475);
#6230=VERTEX_POINT('',#19479);
#6231=VERTEX_POINT('',#19481);
#6232=VERTEX_POINT('',#19485);
#6233=VERTEX_POINT('',#19486);
#6234=VERTEX_POINT('',#19488);
#6235=VERTEX_POINT('',#19490);
#6236=VERTEX_POINT('',#19494);
#6237=VERTEX_POINT('',#19496);
#6238=VERTEX_POINT('',#19500);
#6239=VERTEX_POINT('',#19502);
#6240=VERTEX_POINT('',#19512);
#6241=VERTEX_POINT('',#19513);
#6242=VERTEX_POINT('',#19515);
#6243=VERTEX_POINT('',#19517);
#6244=VERTEX_POINT('',#19521);
#6245=VERTEX_POINT('',#19523);
#6246=VERTEX_POINT('',#19527);
#6247=VERTEX_POINT('',#19529);
#6248=VERTEX_POINT('',#19539);
#6249=VERTEX_POINT('',#19540);
#6250=VERTEX_POINT('',#19542);
#6251=VERTEX_POINT('',#19544);
#6252=VERTEX_POINT('',#19548);
#6253=VERTEX_POINT('',#19550);
#6254=VERTEX_POINT('',#19554);
#6255=VERTEX_POINT('',#19556);
#6256=VERTEX_POINT('',#19566);
#6257=VERTEX_POINT('',#19568);
#6258=VERTEX_POINT('',#19572);
#6259=VERTEX_POINT('',#19574);
#6260=VERTEX_POINT('',#19578);
#6261=VERTEX_POINT('',#19580);
#6262=VERTEX_POINT('',#19584);
#6263=VERTEX_POINT('',#19586);
#6264=VERTEX_POINT('',#19590);
#6265=VERTEX_POINT('',#19592);
#6266=VERTEX_POINT('',#19596);
#6267=VERTEX_POINT('',#19598);
#6268=VERTEX_POINT('',#19602);
#6269=VERTEX_POINT('',#19604);
#6270=VERTEX_POINT('',#19608);
#6271=VERTEX_POINT('',#19610);
#6272=VERTEX_POINT('',#19614);
#6273=VERTEX_POINT('',#19616);
#6274=VERTEX_POINT('',#19620);
#6275=VERTEX_POINT('',#19622);
#6276=VERTEX_POINT('',#19626);
#6277=VERTEX_POINT('',#19628);
#6278=VERTEX_POINT('',#19632);
#6279=VERTEX_POINT('',#19634);
#6280=VERTEX_POINT('',#19638);
#6281=VERTEX_POINT('',#19640);
#6282=VERTEX_POINT('',#19644);
#6283=VERTEX_POINT('',#19646);
#6284=VERTEX_POINT('',#19650);
#6285=VERTEX_POINT('',#19652);
#6286=VERTEX_POINT('',#19656);
#6287=VERTEX_POINT('',#19658);
#6288=VERTEX_POINT('',#19662);
#6289=VERTEX_POINT('',#19663);
#6290=VERTEX_POINT('',#19665);
#6291=VERTEX_POINT('',#19667);
#6292=VERTEX_POINT('',#19671);
#6293=VERTEX_POINT('',#19673);
#6294=VERTEX_POINT('',#19677);
#6295=VERTEX_POINT('',#19679);
#6296=VERTEX_POINT('',#19689);
#6297=VERTEX_POINT('',#19691);
#6298=VERTEX_POINT('',#19695);
#6299=VERTEX_POINT('',#19698);
#6300=VERTEX_POINT('',#19700);
#6301=VERTEX_POINT('',#19704);
#6302=VERTEX_POINT('',#19707);
#6303=VERTEX_POINT('',#19711);
#6304=VERTEX_POINT('',#19715);
#6305=VERTEX_POINT('',#19716);
#6306=VERTEX_POINT('',#19718);
#6307=VERTEX_POINT('',#19720);
#6308=VERTEX_POINT('',#19724);
#6309=VERTEX_POINT('',#19726);
#6310=VERTEX_POINT('',#19730);
#6311=VERTEX_POINT('',#19732);
#6312=VERTEX_POINT('',#19742);
#6313=VERTEX_POINT('',#19743);
#6314=VERTEX_POINT('',#19745);
#6315=VERTEX_POINT('',#19747);
#6316=VERTEX_POINT('',#19751);
#6317=VERTEX_POINT('',#19753);
#6318=VERTEX_POINT('',#19757);
#6319=VERTEX_POINT('',#19759);
#6320=VERTEX_POINT('',#19769);
#6321=VERTEX_POINT('',#19771);
#6322=VERTEX_POINT('',#19775);
#6323=VERTEX_POINT('',#19778);
#6324=VERTEX_POINT('',#19780);
#6325=VERTEX_POINT('',#19784);
#6326=VERTEX_POINT('',#19787);
#6327=VERTEX_POINT('',#19791);
#6328=VERTEX_POINT('',#19795);
#6329=VERTEX_POINT('',#19796);
#6330=VERTEX_POINT('',#19798);
#6331=VERTEX_POINT('',#19800);
#6332=VERTEX_POINT('',#19804);
#6333=VERTEX_POINT('',#19806);
#6334=VERTEX_POINT('',#19810);
#6335=VERTEX_POINT('',#19812);
#6336=VERTEX_POINT('',#19822);
#6337=VERTEX_POINT('',#19823);
#6338=VERTEX_POINT('',#19825);
#6339=VERTEX_POINT('',#19827);
#6340=VERTEX_POINT('',#19831);
#6341=VERTEX_POINT('',#19833);
#6342=VERTEX_POINT('',#19837);
#6343=VERTEX_POINT('',#19839);
#6344=VERTEX_POINT('',#19849);
#6345=VERTEX_POINT('',#19851);
#6346=VERTEX_POINT('',#19855);
#6347=VERTEX_POINT('',#19857);
#6348=VERTEX_POINT('',#19861);
#6349=VERTEX_POINT('',#19863);
#6350=VERTEX_POINT('',#19867);
#6351=VERTEX_POINT('',#19869);
#6352=VERTEX_POINT('',#19873);
#6353=VERTEX_POINT('',#19875);
#6354=VERTEX_POINT('',#19879);
#6355=VERTEX_POINT('',#19881);
#6356=VERTEX_POINT('',#19885);
#6357=VERTEX_POINT('',#19887);
#6358=VERTEX_POINT('',#19891);
#6359=VERTEX_POINT('',#19892);
#6360=VERTEX_POINT('',#19894);
#6361=VERTEX_POINT('',#19896);
#6362=VERTEX_POINT('',#19900);
#6363=VERTEX_POINT('',#19901);
#6364=VERTEX_POINT('',#19903);
#6365=VERTEX_POINT('',#19905);
#6366=VERTEX_POINT('',#19909);
#6367=VERTEX_POINT('',#19911);
#6368=VERTEX_POINT('',#19915);
#6369=VERTEX_POINT('',#19917);
#6370=VERTEX_POINT('',#19921);
#6371=VERTEX_POINT('',#19923);
#6372=VERTEX_POINT('',#19928);
#6373=VERTEX_POINT('',#19932);
#6374=VERTEX_POINT('',#19942);
#6375=VERTEX_POINT('',#19944);
#6376=VERTEX_POINT('',#19948);
#6377=VERTEX_POINT('',#19950);
#6378=VERTEX_POINT('',#19954);
#6379=VERTEX_POINT('',#19956);
#6380=VERTEX_POINT('',#19960);
#6381=VERTEX_POINT('',#19962);
#6382=VERTEX_POINT('',#19966);
#6383=VERTEX_POINT('',#19968);
#6384=VERTEX_POINT('',#19972);
#6385=VERTEX_POINT('',#19975);
#6386=VERTEX_POINT('',#19979);
#6387=VERTEX_POINT('',#19981);
#6388=VERTEX_POINT('',#19988);
#6389=VERTEX_POINT('',#19990);
#6390=VERTEX_POINT('',#19994);
#6391=VERTEX_POINT('',#19996);
#6392=VERTEX_POINT('',#20000);
#6393=VERTEX_POINT('',#20002);
#6394=VERTEX_POINT('',#20006);
#6395=VERTEX_POINT('',#20008);
#6396=VERTEX_POINT('',#20012);
#6397=VERTEX_POINT('',#20014);
#6398=VERTEX_POINT('',#20018);
#6399=VERTEX_POINT('',#20021);
#6400=VERTEX_POINT('',#20025);
#6401=VERTEX_POINT('',#20027);
#6402=VERTEX_POINT('',#20034);
#6403=VERTEX_POINT('',#20036);
#6404=VERTEX_POINT('',#20040);
#6405=VERTEX_POINT('',#20042);
#6406=VERTEX_POINT('',#20046);
#6407=VERTEX_POINT('',#20048);
#6408=VERTEX_POINT('',#20052);
#6409=VERTEX_POINT('',#20054);
#6410=VERTEX_POINT('',#20058);
#6411=VERTEX_POINT('',#20060);
#6412=VERTEX_POINT('',#20064);
#6413=VERTEX_POINT('',#20066);
#6414=VERTEX_POINT('',#20070);
#6415=VERTEX_POINT('',#20072);
#6416=VERTEX_POINT('',#20076);
#6417=VERTEX_POINT('',#20077);
#6418=VERTEX_POINT('',#20079);
#6419=VERTEX_POINT('',#20081);
#6420=VERTEX_POINT('',#20085);
#6421=VERTEX_POINT('',#20086);
#6422=VERTEX_POINT('',#20088);
#6423=VERTEX_POINT('',#20090);
#6424=VERTEX_POINT('',#20094);
#6425=VERTEX_POINT('',#20096);
#6426=VERTEX_POINT('',#20100);
#6427=VERTEX_POINT('',#20102);
#6428=VERTEX_POINT('',#20106);
#6429=VERTEX_POINT('',#20108);
#6430=VERTEX_POINT('',#20113);
#6431=VERTEX_POINT('',#20117);
#6432=VERTEX_POINT('',#20127);
#6433=VERTEX_POINT('',#20129);
#6434=VERTEX_POINT('',#20133);
#6435=VERTEX_POINT('',#20135);
#6436=VERTEX_POINT('',#20139);
#6437=VERTEX_POINT('',#20141);
#6438=VERTEX_POINT('',#20145);
#6439=VERTEX_POINT('',#20147);
#6440=VERTEX_POINT('',#20151);
#6441=VERTEX_POINT('',#20153);
#6442=VERTEX_POINT('',#20157);
#6443=VERTEX_POINT('',#20160);
#6444=VERTEX_POINT('',#20164);
#6445=VERTEX_POINT('',#20166);
#6446=VERTEX_POINT('',#20173);
#6447=VERTEX_POINT('',#20175);
#6448=VERTEX_POINT('',#20179);
#6449=VERTEX_POINT('',#20181);
#6450=VERTEX_POINT('',#20185);
#6451=VERTEX_POINT('',#20187);
#6452=VERTEX_POINT('',#20191);
#6453=VERTEX_POINT('',#20193);
#6454=VERTEX_POINT('',#20197);
#6455=VERTEX_POINT('',#20199);
#6456=VERTEX_POINT('',#20203);
#6457=VERTEX_POINT('',#20206);
#6458=VERTEX_POINT('',#20210);
#6459=VERTEX_POINT('',#20212);
#6460=VERTEX_POINT('',#20219);
#6461=VERTEX_POINT('',#20220);
#6462=VERTEX_POINT('',#20222);
#6463=VERTEX_POINT('',#20224);
#6464=VERTEX_POINT('',#20228);
#6465=VERTEX_POINT('',#20230);
#6466=VERTEX_POINT('',#20234);
#6467=VERTEX_POINT('',#20236);
#6468=VERTEX_POINT('',#20240);
#6469=VERTEX_POINT('',#20242);
#6470=VERTEX_POINT('',#20246);
#6471=VERTEX_POINT('',#20248);
#6472=VERTEX_POINT('',#20252);
#6473=VERTEX_POINT('',#20254);
#6474=VERTEX_POINT('',#20258);
#6475=VERTEX_POINT('',#20260);
#6476=VERTEX_POINT('',#20264);
#6477=VERTEX_POINT('',#20266);
#6478=VERTEX_POINT('',#20270);
#6479=VERTEX_POINT('',#20272);
#6480=VERTEX_POINT('',#20276);
#6481=VERTEX_POINT('',#20277);
#6482=VERTEX_POINT('',#20279);
#6483=VERTEX_POINT('',#20281);
#6484=VERTEX_POINT('',#20285);
#6485=VERTEX_POINT('',#20287);
#6486=VERTEX_POINT('',#20291);
#6487=VERTEX_POINT('',#20293);
#6488=VERTEX_POINT('',#20297);
#6489=VERTEX_POINT('',#20299);
#6490=VERTEX_POINT('',#20303);
#6491=VERTEX_POINT('',#20305);
#6492=VERTEX_POINT('',#20309);
#6493=VERTEX_POINT('',#20311);
#6494=VERTEX_POINT('',#20315);
#6495=VERTEX_POINT('',#20317);
#6496=VERTEX_POINT('',#20321);
#6497=VERTEX_POINT('',#20323);
#6498=VERTEX_POINT('',#20327);
#6499=VERTEX_POINT('',#20329);
#6500=VERTEX_POINT('',#20333);
#6501=VERTEX_POINT('',#20334);
#6502=VERTEX_POINT('',#20336);
#6503=VERTEX_POINT('',#20338);
#6504=VERTEX_POINT('',#20342);
#6505=VERTEX_POINT('',#20344);
#6506=VERTEX_POINT('',#20348);
#6507=VERTEX_POINT('',#20350);
#6508=VERTEX_POINT('',#20354);
#6509=VERTEX_POINT('',#20356);
#6510=VERTEX_POINT('',#20360);
#6511=VERTEX_POINT('',#20362);
#6512=VERTEX_POINT('',#20366);
#6513=VERTEX_POINT('',#20368);
#6514=VERTEX_POINT('',#20372);
#6515=VERTEX_POINT('',#20374);
#6516=VERTEX_POINT('',#20378);
#6517=VERTEX_POINT('',#20380);
#6518=VERTEX_POINT('',#20384);
#6519=VERTEX_POINT('',#20386);
#6520=VERTEX_POINT('',#20390);
#6521=VERTEX_POINT('',#20391);
#6522=VERTEX_POINT('',#20393);
#6523=VERTEX_POINT('',#20395);
#6524=VERTEX_POINT('',#20399);
#6525=VERTEX_POINT('',#20401);
#6526=VERTEX_POINT('',#20405);
#6527=VERTEX_POINT('',#20407);
#6528=VERTEX_POINT('',#20411);
#6529=VERTEX_POINT('',#20413);
#6530=VERTEX_POINT('',#20417);
#6531=VERTEX_POINT('',#20419);
#6532=VERTEX_POINT('',#20423);
#6533=VERTEX_POINT('',#20425);
#6534=VERTEX_POINT('',#20429);
#6535=VERTEX_POINT('',#20431);
#6536=VERTEX_POINT('',#20435);
#6537=VERTEX_POINT('',#20437);
#6538=VERTEX_POINT('',#20441);
#6539=VERTEX_POINT('',#20443);
#6540=VERTEX_POINT('',#20447);
#6541=VERTEX_POINT('',#20449);
#6542=VERTEX_POINT('',#20453);
#6543=VERTEX_POINT('',#20455);
#6544=VERTEX_POINT('',#20459);
#6545=VERTEX_POINT('',#20461);
#6546=VERTEX_POINT('',#20468);
#6547=VERTEX_POINT('',#20470);
#6548=VERTEX_POINT('',#20477);
#6549=VERTEX_POINT('',#20479);
#6550=VERTEX_POINT('',#20492);
#6551=VERTEX_POINT('',#20493);
#6552=VERTEX_POINT('',#20495);
#6553=VERTEX_POINT('',#20497);
#6554=VERTEX_POINT('',#20501);
#6555=VERTEX_POINT('',#20503);
#6556=VERTEX_POINT('',#20507);
#6557=VERTEX_POINT('',#20509);
#6558=VERTEX_POINT('',#20512);
#6559=VERTEX_POINT('',#20515);
#6560=VERTEX_POINT('',#20517);
#6561=VERTEX_POINT('',#20519);
#6562=VERTEX_POINT('',#20521);
#6563=VERTEX_POINT('',#20523);
#6564=VERTEX_POINT('',#20525);
#6565=VERTEX_POINT('',#20529);
#6566=VERTEX_POINT('',#20533);
#6567=VERTEX_POINT('',#20537);
#6568=VERTEX_POINT('',#20539);
#6569=VERTEX_POINT('',#20541);
#6570=VERTEX_POINT('',#20543);
#6571=VERTEX_POINT('',#20549);
#6572=VERTEX_POINT('',#20551);
#6573=VERTEX_POINT('',#20555);
#6574=VERTEX_POINT('',#20558);
#6575=VERTEX_POINT('',#20560);
#6576=VERTEX_POINT('',#20572);
#6577=VERTEX_POINT('',#20574);
#6578=VERTEX_POINT('',#20578);
#6579=VERTEX_POINT('',#20582);
#6580=VERTEX_POINT('',#20585);
#6581=VERTEX_POINT('',#20591);
#6582=VERTEX_POINT('',#20593);
#6583=VERTEX_POINT('',#20597);
#6584=VERTEX_POINT('',#20600);
#6585=VERTEX_POINT('',#20602);
#6586=VERTEX_POINT('',#20606);
#6587=VERTEX_POINT('',#20609);
#6588=VERTEX_POINT('',#20611);
#6589=VERTEX_POINT('',#20615);
#6590=VERTEX_POINT('',#20618);
#6591=VERTEX_POINT('',#20620);
#6592=VERTEX_POINT('',#20624);
#6593=VERTEX_POINT('',#20627);
#6594=VERTEX_POINT('',#20631);
#6595=VERTEX_POINT('',#20635);
#6596=VERTEX_POINT('',#20639);
#6597=VERTEX_POINT('',#20643);
#6598=VERTEX_POINT('',#20644);
#6599=VERTEX_POINT('',#20646);
#6600=VERTEX_POINT('',#20648);
#6601=VERTEX_POINT('',#20652);
#6602=VERTEX_POINT('',#20654);
#6603=VERTEX_POINT('',#20658);
#6604=VERTEX_POINT('',#20660);
#6605=VERTEX_POINT('',#20664);
#6606=VERTEX_POINT('',#20666);
#6607=VERTEX_POINT('',#20670);
#6608=VERTEX_POINT('',#20672);
#6609=VERTEX_POINT('',#20676);
#6610=VERTEX_POINT('',#20678);
#6611=VERTEX_POINT('',#20682);
#6612=VERTEX_POINT('',#20684);
#6613=VERTEX_POINT('',#20688);
#6614=VERTEX_POINT('',#20690);
#6615=VERTEX_POINT('',#20694);
#6616=VERTEX_POINT('',#20696);
#6617=VERTEX_POINT('',#20700);
#6618=VERTEX_POINT('',#20702);
#6619=VERTEX_POINT('',#20706);
#6620=VERTEX_POINT('',#20708);
#6621=VERTEX_POINT('',#20718);
#6622=VERTEX_POINT('',#20721);
#6623=VERTEX_POINT('',#20725);
#6624=VERTEX_POINT('',#20729);
#6625=VERTEX_POINT('',#20733);
#6626=VERTEX_POINT('',#20736);
#6627=VERTEX_POINT('',#20740);
#6628=VERTEX_POINT('',#20744);
#6629=VERTEX_POINT('',#20749);
#6630=VERTEX_POINT('',#20750);
#6631=VERTEX_POINT('',#20752);
#6632=VERTEX_POINT('',#20754);
#6633=VERTEX_POINT('',#20758);
#6634=VERTEX_POINT('',#20760);
#6635=VERTEX_POINT('',#20764);
#6636=VERTEX_POINT('',#20766);
#6637=VERTEX_POINT('',#20770);
#6638=VERTEX_POINT('',#20772);
#6639=VERTEX_POINT('',#20776);
#6640=VERTEX_POINT('',#20778);
#6641=VERTEX_POINT('',#20789);
#6642=VERTEX_POINT('',#20790);
#6643=VERTEX_POINT('',#20793);
#6644=VERTEX_POINT('',#20795);
#6645=VERTEX_POINT('',#20799);
#6646=VERTEX_POINT('',#20803);
#6647=VERTEX_POINT('',#20805);
#6648=VERTEX_POINT('',#20809);
#6649=VERTEX_POINT('',#20814);
#6650=VERTEX_POINT('',#20818);
#6651=VERTEX_POINT('',#20824);
#6652=VERTEX_POINT('',#20825);
#6653=VERTEX_POINT('',#20828);
#6654=VERTEX_POINT('',#20830);
#6655=VERTEX_POINT('',#20834);
#6656=VERTEX_POINT('',#20838);
#6657=VERTEX_POINT('',#20840);
#6658=VERTEX_POINT('',#20843);
#6659=VERTEX_POINT('',#20847);
#6660=VERTEX_POINT('',#20851);
#6661=VERTEX_POINT('',#20859);
#6662=VERTEX_POINT('',#20860);
#6663=VERTEX_POINT('',#20863);
#6664=VERTEX_POINT('',#20864);
#6665=VERTEX_POINT('',#20867);
#6666=VERTEX_POINT('',#20868);
#6667=VERTEX_POINT('',#20871);
#6668=VERTEX_POINT('',#20872);
#6669=VERTEX_POINT('',#20875);
#6670=VERTEX_POINT('',#20876);
#6671=VERTEX_POINT('',#20879);
#6672=VERTEX_POINT('',#20880);
#6673=VERTEX_POINT('',#20883);
#6674=VERTEX_POINT('',#20884);
#6675=VERTEX_POINT('',#20888);
#6676=VERTEX_POINT('',#20889);
#6677=VERTEX_POINT('',#20912);
#6678=VERTEX_POINT('',#20914);
#6679=VERTEX_POINT('',#20939);
#6680=VERTEX_POINT('',#20941);
#6681=VERTEX_POINT('',#20964);
#6682=VERTEX_POINT('',#20966);
#6683=VERTEX_POINT('',#20989);
#6684=VERTEX_POINT('',#20991);
#6685=VERTEX_POINT('',#20994);
#6686=VERTEX_POINT('',#20996);
#6687=VERTEX_POINT('',#21019);
#6688=VERTEX_POINT('',#21021);
#6689=VERTEX_POINT('',#21044);
#6690=VERTEX_POINT('',#21046);
#6691=VERTEX_POINT('',#21069);
#6692=VERTEX_POINT('',#21071);
#6693=VERTEX_POINT('',#21096);
#6694=VERTEX_POINT('',#21100);
#6695=VERTEX_POINT('',#21125);
#6696=VERTEX_POINT('',#21129);
#6697=VERTEX_POINT('',#21154);
#6698=VERTEX_POINT('',#21156);
#6699=VERTEX_POINT('',#21160);
#6700=VERTEX_POINT('',#21185);
#6701=VERTEX_POINT('',#21189);
#6702=VERTEX_POINT('',#21214);
#6703=VERTEX_POINT('',#21218);
#6704=VERTEX_POINT('',#21243);
#6705=VERTEX_POINT('',#21246);
#6706=VERTEX_POINT('',#21248);
#6707=VERTEX_POINT('',#21280);
#6708=VERTEX_POINT('',#21282);
#6709=VERTEX_POINT('',#21285);
#6710=VERTEX_POINT('',#21289);
#6711=VERTEX_POINT('',#21294);
#6712=VERTEX_POINT('',#21296);
#6713=VERTEX_POINT('',#21299);
#6714=VERTEX_POINT('',#21303);
#6715=VERTEX_POINT('',#21314);
#6716=VERTEX_POINT('',#21315);
#6717=VERTEX_POINT('',#21317);
#6718=VERTEX_POINT('',#21319);
#6719=VERTEX_POINT('',#21323);
#6720=VERTEX_POINT('',#21325);
#6721=VERTEX_POINT('',#21329);
#6722=VERTEX_POINT('',#21331);
#6723=VERTEX_POINT('',#21335);
#6724=VERTEX_POINT('',#21337);
#6725=VERTEX_POINT('',#21341);
#6726=VERTEX_POINT('',#21343);
#6727=VERTEX_POINT('',#21352);
#6728=VERTEX_POINT('',#21355);
#6729=VERTEX_POINT('',#21358);
#6730=VERTEX_POINT('',#21362);
#6731=VERTEX_POINT('',#21366);
#6732=VERTEX_POINT('',#21370);
#6733=VERTEX_POINT('',#21373);
#6734=VERTEX_POINT('',#21381);
#6735=VERTEX_POINT('',#21383);
#6736=VERTEX_POINT('',#21387);
#6737=VERTEX_POINT('',#21389);
#6738=VERTEX_POINT('',#21393);
#6739=VERTEX_POINT('',#21395);
#6740=VERTEX_POINT('',#21399);
#6741=VERTEX_POINT('',#21401);
#6742=VERTEX_POINT('',#21405);
#6743=VERTEX_POINT('',#21407);
#6744=VERTEX_POINT('',#21411);
#6745=VERTEX_POINT('',#21413);
#6746=VERTEX_POINT('',#21417);
#6747=VERTEX_POINT('',#21419);
#6748=VERTEX_POINT('',#21423);
#6749=VERTEX_POINT('',#21425);
#6750=VERTEX_POINT('',#21429);
#6751=VERTEX_POINT('',#21430);
#6752=VERTEX_POINT('',#21432);
#6753=VERTEX_POINT('',#21434);
#6754=VERTEX_POINT('',#21438);
#6755=VERTEX_POINT('',#21440);
#6756=VERTEX_POINT('',#21444);
#6757=VERTEX_POINT('',#21446);
#6758=VERTEX_POINT('',#21456);
#6759=VERTEX_POINT('',#21458);
#6760=VERTEX_POINT('',#21463);
#6761=VERTEX_POINT('',#21465);
#6762=VERTEX_POINT('',#21470);
#6763=VERTEX_POINT('',#21472);
#6764=VERTEX_POINT('',#21477);
#6765=VERTEX_POINT('',#21479);
#6766=VERTEX_POINT('',#21484);
#6767=VERTEX_POINT('',#21485);
#6768=VERTEX_POINT('',#21487);
#6769=VERTEX_POINT('',#21489);
#6770=VERTEX_POINT('',#21493);
#6771=VERTEX_POINT('',#21495);
#6772=VERTEX_POINT('',#21499);
#6773=VERTEX_POINT('',#21501);
#6774=VERTEX_POINT('',#21505);
#6775=VERTEX_POINT('',#21507);
#6776=VERTEX_POINT('',#21511);
#6777=VERTEX_POINT('',#21513);
#6778=VERTEX_POINT('',#21517);
#6779=VERTEX_POINT('',#21519);
#6780=VERTEX_POINT('',#21523);
#6781=VERTEX_POINT('',#21525);
#6782=VERTEX_POINT('',#21529);
#6783=VERTEX_POINT('',#21531);
#6784=VERTEX_POINT('',#21535);
#6785=VERTEX_POINT('',#21537);
#6786=VERTEX_POINT('',#21541);
#6787=VERTEX_POINT('',#21543);
#6788=VERTEX_POINT('',#21547);
#6789=VERTEX_POINT('',#21549);
#6790=VERTEX_POINT('',#21553);
#6791=VERTEX_POINT('',#21555);
#6792=VERTEX_POINT('',#21559);
#6793=VERTEX_POINT('',#21561);
#6794=VERTEX_POINT('',#21565);
#6795=VERTEX_POINT('',#21567);
#6796=VERTEX_POINT('',#21571);
#6797=VERTEX_POINT('',#21573);
#6798=VERTEX_POINT('',#21577);
#6799=VERTEX_POINT('',#21579);
#6800=VERTEX_POINT('',#21583);
#6801=VERTEX_POINT('',#21585);
#6802=VERTEX_POINT('',#21589);
#6803=VERTEX_POINT('',#21591);
#6804=VERTEX_POINT('',#21595);
#6805=VERTEX_POINT('',#21597);
#6806=VERTEX_POINT('',#21601);
#6807=VERTEX_POINT('',#21603);
#6808=VERTEX_POINT('',#21607);
#6809=VERTEX_POINT('',#21609);
#6810=VERTEX_POINT('',#21613);
#6811=VERTEX_POINT('',#21615);
#6812=VERTEX_POINT('',#21619);
#6813=VERTEX_POINT('',#21621);
#6814=VERTEX_POINT('',#21625);
#6815=VERTEX_POINT('',#21627);
#6816=VERTEX_POINT('',#21631);
#6817=VERTEX_POINT('',#21633);
#6818=VERTEX_POINT('',#21637);
#6819=VERTEX_POINT('',#21639);
#6820=VERTEX_POINT('',#21643);
#6821=VERTEX_POINT('',#21645);
#6822=VERTEX_POINT('',#21649);
#6823=VERTEX_POINT('',#21651);
#6824=VERTEX_POINT('',#21655);
#6825=VERTEX_POINT('',#21657);
#6826=VERTEX_POINT('',#21661);
#6827=VERTEX_POINT('',#21663);
#6828=VERTEX_POINT('',#21667);
#6829=VERTEX_POINT('',#21669);
#6830=VERTEX_POINT('',#21673);
#6831=VERTEX_POINT('',#21675);
#6832=VERTEX_POINT('',#21679);
#6833=VERTEX_POINT('',#21681);
#6834=VERTEX_POINT('',#21685);
#6835=VERTEX_POINT('',#21687);
#6836=VERTEX_POINT('',#21691);
#6837=VERTEX_POINT('',#21693);
#6838=VERTEX_POINT('',#21697);
#6839=VERTEX_POINT('',#21699);
#6840=VERTEX_POINT('',#21703);
#6841=VERTEX_POINT('',#21705);
#6842=VERTEX_POINT('',#21709);
#6843=VERTEX_POINT('',#21711);
#6844=VERTEX_POINT('',#21715);
#6845=VERTEX_POINT('',#21717);
#6846=VERTEX_POINT('',#21721);
#6847=VERTEX_POINT('',#21723);
#6848=VERTEX_POINT('',#21727);
#6849=VERTEX_POINT('',#21729);
#6850=VERTEX_POINT('',#21733);
#6851=VERTEX_POINT('',#21735);
#6852=VERTEX_POINT('',#21739);
#6853=VERTEX_POINT('',#21741);
#6854=VERTEX_POINT('',#21745);
#6855=VERTEX_POINT('',#21747);
#6856=VERTEX_POINT('',#21751);
#6857=VERTEX_POINT('',#21753);
#6858=VERTEX_POINT('',#21757);
#6859=VERTEX_POINT('',#21759);
#6860=VERTEX_POINT('',#21763);
#6861=VERTEX_POINT('',#21765);
#6862=VERTEX_POINT('',#21769);
#6863=VERTEX_POINT('',#21771);
#6864=VERTEX_POINT('',#21775);
#6865=VERTEX_POINT('',#21777);
#6866=VERTEX_POINT('',#21781);
#6867=VERTEX_POINT('',#21783);
#6868=VERTEX_POINT('',#21787);
#6869=VERTEX_POINT('',#21789);
#6870=VERTEX_POINT('',#21793);
#6871=VERTEX_POINT('',#21795);
#6872=VERTEX_POINT('',#21799);
#6873=VERTEX_POINT('',#21801);
#6874=VERTEX_POINT('',#21805);
#6875=VERTEX_POINT('',#21807);
#6876=VERTEX_POINT('',#21811);
#6877=VERTEX_POINT('',#21813);
#6878=VERTEX_POINT('',#21817);
#6879=VERTEX_POINT('',#21819);
#6880=VERTEX_POINT('',#21823);
#6881=VERTEX_POINT('',#21825);
#6882=VERTEX_POINT('',#21829);
#6883=VERTEX_POINT('',#21831);
#6884=VERTEX_POINT('',#21835);
#6885=VERTEX_POINT('',#21837);
#6886=VERTEX_POINT('',#21841);
#6887=VERTEX_POINT('',#21843);
#6888=VERTEX_POINT('',#21847);
#6889=VERTEX_POINT('',#21849);
#6890=VERTEX_POINT('',#21853);
#6891=VERTEX_POINT('',#21855);
#6892=VERTEX_POINT('',#21859);
#6893=VERTEX_POINT('',#21861);
#6894=VERTEX_POINT('',#21865);
#6895=VERTEX_POINT('',#21867);
#6896=VERTEX_POINT('',#21871);
#6897=VERTEX_POINT('',#21873);
#6898=VERTEX_POINT('',#21877);
#6899=VERTEX_POINT('',#21879);
#6900=VERTEX_POINT('',#21883);
#6901=VERTEX_POINT('',#21885);
#6902=VERTEX_POINT('',#21889);
#6903=VERTEX_POINT('',#21891);
#6904=VERTEX_POINT('',#21895);
#6905=VERTEX_POINT('',#21897);
#6906=VERTEX_POINT('',#21901);
#6907=VERTEX_POINT('',#21903);
#6908=VERTEX_POINT('',#21907);
#6909=VERTEX_POINT('',#21909);
#6910=VERTEX_POINT('',#21913);
#6911=VERTEX_POINT('',#21915);
#6912=VERTEX_POINT('',#21919);
#6913=VERTEX_POINT('',#21921);
#6914=VERTEX_POINT('',#21925);
#6915=VERTEX_POINT('',#21927);
#6916=VERTEX_POINT('',#21931);
#6917=VERTEX_POINT('',#21933);
#6918=VERTEX_POINT('',#21937);
#6919=VERTEX_POINT('',#21939);
#6920=VERTEX_POINT('',#21943);
#6921=VERTEX_POINT('',#21945);
#6922=VERTEX_POINT('',#21949);
#6923=VERTEX_POINT('',#21951);
#6924=VERTEX_POINT('',#21955);
#6925=VERTEX_POINT('',#21957);
#6926=VERTEX_POINT('',#21961);
#6927=VERTEX_POINT('',#21963);
#6928=VERTEX_POINT('',#21967);
#6929=VERTEX_POINT('',#21969);
#6930=VERTEX_POINT('',#21973);
#6931=VERTEX_POINT('',#21975);
#6932=VERTEX_POINT('',#21979);
#6933=VERTEX_POINT('',#21981);
#6934=VERTEX_POINT('',#21985);
#6935=VERTEX_POINT('',#21987);
#6936=VERTEX_POINT('',#21991);
#6937=VERTEX_POINT('',#21993);
#6938=VERTEX_POINT('',#21997);
#6939=VERTEX_POINT('',#21999);
#6940=VERTEX_POINT('',#22003);
#6941=VERTEX_POINT('',#22005);
#6942=VERTEX_POINT('',#22009);
#6943=VERTEX_POINT('',#22011);
#6944=VERTEX_POINT('',#22015);
#6945=VERTEX_POINT('',#22017);
#6946=VERTEX_POINT('',#22021);
#6947=VERTEX_POINT('',#22023);
#6948=VERTEX_POINT('',#22027);
#6949=VERTEX_POINT('',#22029);
#6950=VERTEX_POINT('',#22033);
#6951=VERTEX_POINT('',#22035);
#6952=VERTEX_POINT('',#22039);
#6953=VERTEX_POINT('',#22041);
#6954=VERTEX_POINT('',#22045);
#6955=VERTEX_POINT('',#22047);
#6956=VERTEX_POINT('',#22051);
#6957=VERTEX_POINT('',#22053);
#6958=VERTEX_POINT('',#22057);
#6959=VERTEX_POINT('',#22059);
#6960=VERTEX_POINT('',#22063);
#6961=VERTEX_POINT('',#22065);
#6962=VERTEX_POINT('',#22069);
#6963=VERTEX_POINT('',#22071);
#6964=VERTEX_POINT('',#22075);
#6965=VERTEX_POINT('',#22077);
#6966=VERTEX_POINT('',#22081);
#6967=VERTEX_POINT('',#22083);
#6968=VERTEX_POINT('',#22087);
#6969=VERTEX_POINT('',#22089);
#6970=VERTEX_POINT('',#22093);
#6971=VERTEX_POINT('',#22095);
#6972=VERTEX_POINT('',#22099);
#6973=VERTEX_POINT('',#22101);
#6974=VERTEX_POINT('',#22105);
#6975=VERTEX_POINT('',#22107);
#6976=VERTEX_POINT('',#22111);
#6977=VERTEX_POINT('',#22113);
#6978=VERTEX_POINT('',#22117);
#6979=VERTEX_POINT('',#22119);
#6980=VERTEX_POINT('',#22123);
#6981=VERTEX_POINT('',#22125);
#6982=VERTEX_POINT('',#22129);
#6983=VERTEX_POINT('',#22131);
#6984=VERTEX_POINT('',#22135);
#6985=VERTEX_POINT('',#22137);
#6986=VERTEX_POINT('',#22141);
#6987=VERTEX_POINT('',#22143);
#6988=VERTEX_POINT('',#22147);
#6989=VERTEX_POINT('',#22149);
#6990=VERTEX_POINT('',#22153);
#6991=VERTEX_POINT('',#22155);
#6992=VERTEX_POINT('',#22159);
#6993=VERTEX_POINT('',#22161);
#6994=VERTEX_POINT('',#22165);
#6995=VERTEX_POINT('',#22167);
#6996=VERTEX_POINT('',#22171);
#6997=VERTEX_POINT('',#22173);
#6998=VERTEX_POINT('',#22177);
#6999=VERTEX_POINT('',#22179);
#7000=VERTEX_POINT('',#22183);
#7001=VERTEX_POINT('',#22185);
#7002=VERTEX_POINT('',#22189);
#7003=VERTEX_POINT('',#22191);
#7004=VERTEX_POINT('',#22195);
#7005=VERTEX_POINT('',#22197);
#7006=VERTEX_POINT('',#22201);
#7007=VERTEX_POINT('',#22203);
#7008=VERTEX_POINT('',#22207);
#7009=VERTEX_POINT('',#22209);
#7010=VERTEX_POINT('',#22213);
#7011=VERTEX_POINT('',#22215);
#7012=VERTEX_POINT('',#22219);
#7013=VERTEX_POINT('',#22221);
#7014=VERTEX_POINT('',#22225);
#7015=VERTEX_POINT('',#22227);
#7016=VERTEX_POINT('',#22231);
#7017=VERTEX_POINT('',#22233);
#7018=VERTEX_POINT('',#22237);
#7019=VERTEX_POINT('',#22239);
#7020=VERTEX_POINT('',#22243);
#7021=VERTEX_POINT('',#22245);
#7022=VERTEX_POINT('',#22256);
#7023=VERTEX_POINT('',#22257);
#7024=VERTEX_POINT('',#22261);
#7025=VERTEX_POINT('',#22263);
#7026=VERTEX_POINT('',#22265);
#7027=VERTEX_POINT('',#22268);
#7028=VERTEX_POINT('',#22272);
#7029=VERTEX_POINT('',#22273);
#7030=VERTEX_POINT('',#22277);
#7031=VERTEX_POINT('',#22279);
#7032=VERTEX_POINT('',#22281);
#7033=VERTEX_POINT('',#22284);
#7034=VERTEX_POINT('',#22288);
#7035=VERTEX_POINT('',#22289);
#7036=VERTEX_POINT('',#22293);
#7037=VERTEX_POINT('',#22295);
#7038=VERTEX_POINT('',#22297);
#7039=VERTEX_POINT('',#22300);
#7040=VERTEX_POINT('',#22304);
#7041=VERTEX_POINT('',#22305);
#7042=VERTEX_POINT('',#22309);
#7043=VERTEX_POINT('',#22311);
#7044=VERTEX_POINT('',#22313);
#7045=VERTEX_POINT('',#22316);
#7046=VERTEX_POINT('',#22321);
#7047=VERTEX_POINT('',#22323);
#7048=VERTEX_POINT('',#22325);
#7049=VERTEX_POINT('',#22327);
#7050=VERTEX_POINT('',#22332);
#7051=VERTEX_POINT('',#22334);
#7052=VERTEX_POINT('',#22336);
#7053=VERTEX_POINT('',#22338);
#7054=VERTEX_POINT('',#22342);
#7055=VERTEX_POINT('',#22344);
#7056=VERTEX_POINT('',#22346);
#7057=VERTEX_POINT('',#22348);
#7058=VERTEX_POINT('',#22351);
#7059=VERTEX_POINT('',#22353);
#7060=VERTEX_POINT('',#22355);
#7061=VERTEX_POINT('',#22357);
#7062=VERTEX_POINT('',#22361);
#7063=VERTEX_POINT('',#22365);
#7064=VERTEX_POINT('',#22369);
#7065=VERTEX_POINT('',#22373);
#7066=VERTEX_POINT('',#22379);
#7067=VERTEX_POINT('',#22383);
#7068=VERTEX_POINT('',#22387);
#7069=VERTEX_POINT('',#22391);
#7070=VERTEX_POINT('',#22399);
#7071=VERTEX_POINT('',#22400);
#7072=VERTEX_POINT('',#22402);
#7073=VERTEX_POINT('',#22404);
#7074=VERTEX_POINT('',#22408);
#7075=VERTEX_POINT('',#22410);
#7076=VERTEX_POINT('',#22414);
#7077=VERTEX_POINT('',#22416);
#7078=VERTEX_POINT('',#22420);
#7079=VERTEX_POINT('',#22422);
#7080=VERTEX_POINT('',#22426);
#7081=VERTEX_POINT('',#22428);
#7082=VERTEX_POINT('',#22432);
#7083=VERTEX_POINT('',#22434);
#7084=VERTEX_POINT('',#22438);
#7085=VERTEX_POINT('',#22440);
#7086=VERTEX_POINT('',#22450);
#7087=VERTEX_POINT('',#22451);
#7088=VERTEX_POINT('',#22453);
#7089=VERTEX_POINT('',#22455);
#7090=VERTEX_POINT('',#22459);
#7091=VERTEX_POINT('',#22461);
#7092=VERTEX_POINT('',#22465);
#7093=VERTEX_POINT('',#22467);
#7094=VERTEX_POINT('',#22471);
#7095=VERTEX_POINT('',#22473);
#7096=VERTEX_POINT('',#22477);
#7097=VERTEX_POINT('',#22479);
#7098=VERTEX_POINT('',#22483);
#7099=VERTEX_POINT('',#22485);
#7100=VERTEX_POINT('',#22489);
#7101=VERTEX_POINT('',#22491);
#7102=VERTEX_POINT('',#22504);
#7103=VERTEX_POINT('',#22505);
#7104=VERTEX_POINT('',#22507);
#7105=VERTEX_POINT('',#22509);
#7106=VERTEX_POINT('',#22513);
#7107=VERTEX_POINT('',#22515);
#7108=VERTEX_POINT('',#22519);
#7109=VERTEX_POINT('',#22521);
#7110=VERTEX_POINT('',#22525);
#7111=VERTEX_POINT('',#22527);
#7112=VERTEX_POINT('',#22531);
#7113=VERTEX_POINT('',#22533);
#7114=VERTEX_POINT('',#22542);
#7115=VERTEX_POINT('',#22545);
#7116=VERTEX_POINT('',#22548);
#7117=VERTEX_POINT('',#22552);
#7118=VERTEX_POINT('',#22556);
#7119=VERTEX_POINT('',#22560);
#7120=VERTEX_POINT('',#22563);
#7121=VERTEX_POINT('',#22571);
#7122=VERTEX_POINT('',#22572);
#7123=VERTEX_POINT('',#22574);
#7124=VERTEX_POINT('',#22576);
#7125=VERTEX_POINT('',#22580);
#7126=VERTEX_POINT('',#22582);
#7127=VERTEX_POINT('',#22586);
#7128=VERTEX_POINT('',#22588);
#7129=VERTEX_POINT('',#22596);
#7130=VERTEX_POINT('',#22598);
#7131=VERTEX_POINT('',#22603);
#7132=VERTEX_POINT('',#22605);
#7133=VERTEX_POINT('',#22610);
#7134=VERTEX_POINT('',#22611);
#7135=VERTEX_POINT('',#22613);
#7136=VERTEX_POINT('',#22615);
#7137=VERTEX_POINT('',#22619);
#7138=VERTEX_POINT('',#22621);
#7139=VERTEX_POINT('',#22625);
#7140=VERTEX_POINT('',#22627);
#7141=VERTEX_POINT('',#22635);
#7142=VERTEX_POINT('',#22637);
#7143=VERTEX_POINT('',#22640);
#7144=VERTEX_POINT('',#22642);
#7145=VERTEX_POINT('',#22647);
#7146=VERTEX_POINT('',#22651);
#7147=VERTEX_POINT('',#22658);
#7148=VERTEX_POINT('',#22660);
#7149=VERTEX_POINT('',#22664);
#7150=VERTEX_POINT('',#22666);
#7151=VERTEX_POINT('',#22673);
#7152=VERTEX_POINT('',#22675);
#7153=VERTEX_POINT('',#22679);
#7154=VERTEX_POINT('',#22681);
#7155=VERTEX_POINT('',#22688);
#7156=VERTEX_POINT('',#22690);
#7157=VERTEX_POINT('',#22694);
#7158=VERTEX_POINT('',#22696);
#7159=VERTEX_POINT('',#22703);
#7160=VERTEX_POINT('',#22705);
#7161=VERTEX_POINT('',#22709);
#7162=VERTEX_POINT('',#22711);
#7163=VERTEX_POINT('',#22718);
#7164=VERTEX_POINT('',#22720);
#7165=VERTEX_POINT('',#22724);
#7166=VERTEX_POINT('',#22726);
#7167=VERTEX_POINT('',#22733);
#7168=VERTEX_POINT('',#22735);
#7169=VERTEX_POINT('',#22739);
#7170=VERTEX_POINT('',#22741);
#7171=VERTEX_POINT('',#22748);
#7172=VERTEX_POINT('',#22750);
#7173=VERTEX_POINT('',#22754);
#7174=VERTEX_POINT('',#22755);
#7175=VERTEX_POINT('',#22757);
#7176=VERTEX_POINT('',#22759);
#7177=VERTEX_POINT('',#22763);
#7178=VERTEX_POINT('',#22765);
#7179=VERTEX_POINT('',#22769);
#7180=VERTEX_POINT('',#22771);
#7181=VERTEX_POINT('',#22775);
#7182=VERTEX_POINT('',#22781);
#7183=VERTEX_POINT('',#22782);
#7184=VERTEX_POINT('',#22784);
#7185=VERTEX_POINT('',#22786);
#7186=VERTEX_POINT('',#22790);
#7187=VERTEX_POINT('',#22792);
#7188=VERTEX_POINT('',#22796);
#7189=VERTEX_POINT('',#22800);
#7190=VERTEX_POINT('',#22806);
#7191=VERTEX_POINT('',#22812);
#7192=VERTEX_POINT('',#22814);
#7193=VERTEX_POINT('',#22818);
#7194=VERTEX_POINT('',#22820);
#7195=VERTEX_POINT('',#22827);
#7196=VERTEX_POINT('',#22828);
#7197=VERTEX_POINT('',#22830);
#7198=VERTEX_POINT('',#22832);
#7199=VERTEX_POINT('',#22836);
#7200=VERTEX_POINT('',#22838);
#7201=VERTEX_POINT('',#22842);
#7202=VERTEX_POINT('',#22844);
#7203=VERTEX_POINT('',#22848);
#7204=VERTEX_POINT('',#22849);
#7205=VERTEX_POINT('',#22851);
#7206=VERTEX_POINT('',#22922);
#7207=VERTEX_POINT('',#22924);
#7208=VERTEX_POINT('',#22995);
#7209=VERTEX_POINT('',#22997);
#7210=VERTEX_POINT('',#23068);
#7211=VERTEX_POINT('',#23070);
#7212=VERTEX_POINT('',#23141);
#7213=VERTEX_POINT('',#23143);
#7214=VERTEX_POINT('',#23214);
#7215=VERTEX_POINT('',#23216);
#7216=VERTEX_POINT('',#23287);
#7217=VERTEX_POINT('',#23289);
#7218=VERTEX_POINT('',#23360);
#7219=VERTEX_POINT('',#23362);
#7220=VERTEX_POINT('',#23433);
#7221=VERTEX_POINT('',#23435);
#7222=VERTEX_POINT('',#23506);
#7223=VERTEX_POINT('',#23508);
#7224=VERTEX_POINT('',#23579);
#7225=VERTEX_POINT('',#23581);
#7226=VERTEX_POINT('',#23652);
#7227=VERTEX_POINT('',#23654);
#7228=VERTEX_POINT('',#23725);
#7229=VERTEX_POINT('',#23727);
#7230=VERTEX_POINT('',#23798);
#7231=VERTEX_POINT('',#23800);
#7232=VERTEX_POINT('',#23871);
#7233=VERTEX_POINT('',#23873);
#7234=VERTEX_POINT('',#23944);
#7235=VERTEX_POINT('',#23946);
#7236=VERTEX_POINT('',#24017);
#7237=VERTEX_POINT('',#24019);
#7238=VERTEX_POINT('',#24090);
#7239=VERTEX_POINT('',#24092);
#7240=VERTEX_POINT('',#24163);
#7241=VERTEX_POINT('',#24165);
#7242=VERTEX_POINT('',#24236);
#7243=VERTEX_POINT('',#24238);
#7244=VERTEX_POINT('',#24309);
#7245=VERTEX_POINT('',#24311);
#7246=VERTEX_POINT('',#24382);
#7247=VERTEX_POINT('',#24384);
#7248=VERTEX_POINT('',#24455);
#7249=VERTEX_POINT('',#24457);
#7250=VERTEX_POINT('',#24528);
#7251=VERTEX_POINT('',#24530);
#7252=VERTEX_POINT('',#24601);
#7253=VERTEX_POINT('',#24603);
#7254=VERTEX_POINT('',#24674);
#7255=VERTEX_POINT('',#24676);
#7256=VERTEX_POINT('',#24747);
#7257=VERTEX_POINT('',#24749);
#7258=VERTEX_POINT('',#24820);
#7259=VERTEX_POINT('',#24822);
#7260=VERTEX_POINT('',#24893);
#7261=VERTEX_POINT('',#24895);
#7262=VERTEX_POINT('',#24966);
#7263=VERTEX_POINT('',#24968);
#7264=VERTEX_POINT('',#25039);
#7265=VERTEX_POINT('',#25041);
#7266=VERTEX_POINT('',#25112);
#7267=VERTEX_POINT('',#25114);
#7268=VERTEX_POINT('',#25185);
#7269=VERTEX_POINT('',#25187);
#7270=VERTEX_POINT('',#25258);
#7271=VERTEX_POINT('',#25260);
#7272=VERTEX_POINT('',#25331);
#7273=VERTEX_POINT('',#25333);
#7274=VERTEX_POINT('',#25404);
#7275=VERTEX_POINT('',#25406);
#7276=VERTEX_POINT('',#25477);
#7277=VERTEX_POINT('',#25479);
#7278=VERTEX_POINT('',#25550);
#7279=VERTEX_POINT('',#25552);
#7280=VERTEX_POINT('',#25623);
#7281=VERTEX_POINT('',#25625);
#7282=VERTEX_POINT('',#25696);
#7283=VERTEX_POINT('',#25772);
#7284=VERTEX_POINT('',#25774);
#7285=VERTEX_POINT('',#25918);
#7286=VERTEX_POINT('',#25920);
#7287=VERTEX_POINT('',#25993);
#7288=VERTEX_POINT('',#26136);
#7289=VERTEX_POINT('',#26209);
#7290=VERTEX_POINT('',#26352);
#7291=VERTEX_POINT('',#26425);
#7292=VERTEX_POINT('',#26568);
#7293=VERTEX_POINT('',#26641);
#7294=VERTEX_POINT('',#26784);
#7295=VERTEX_POINT('',#26857);
#7296=VERTEX_POINT('',#27000);
#7297=VERTEX_POINT('',#27073);
#7298=VERTEX_POINT('',#27216);
#7299=VERTEX_POINT('',#27289);
#7300=VERTEX_POINT('',#27432);
#7301=VERTEX_POINT('',#27505);
#7302=VERTEX_POINT('',#27648);
#7303=VERTEX_POINT('',#27721);
#7304=VERTEX_POINT('',#27864);
#7305=VERTEX_POINT('',#27937);
#7306=VERTEX_POINT('',#28080);
#7307=VERTEX_POINT('',#28153);
#7308=VERTEX_POINT('',#28296);
#7309=VERTEX_POINT('',#28369);
#7310=VERTEX_POINT('',#28512);
#7311=VERTEX_POINT('',#28585);
#7312=VERTEX_POINT('',#28728);
#7313=VERTEX_POINT('',#28801);
#7314=VERTEX_POINT('',#28944);
#7315=VERTEX_POINT('',#29017);
#7316=VERTEX_POINT('',#29160);
#7317=VERTEX_POINT('',#29233);
#7318=VERTEX_POINT('',#29376);
#7319=VERTEX_POINT('',#29449);
#7320=VERTEX_POINT('',#29592);
#7321=VERTEX_POINT('',#29665);
#7322=VERTEX_POINT('',#29808);
#7323=VERTEX_POINT('',#29881);
#7324=VERTEX_POINT('',#30024);
#7325=VERTEX_POINT('',#30097);
#7326=VERTEX_POINT('',#30240);
#7327=VERTEX_POINT('',#30313);
#7328=VERTEX_POINT('',#30456);
#7329=VERTEX_POINT('',#30529);
#7330=VERTEX_POINT('',#30672);
#7331=VERTEX_POINT('',#30745);
#7332=VERTEX_POINT('',#30888);
#7333=VERTEX_POINT('',#30961);
#7334=VERTEX_POINT('',#31104);
#7335=VERTEX_POINT('',#31177);
#7336=VERTEX_POINT('',#31320);
#7337=VERTEX_POINT('',#31393);
#7338=VERTEX_POINT('',#31536);
#7339=VERTEX_POINT('',#31609);
#7340=VERTEX_POINT('',#31752);
#7341=VERTEX_POINT('',#31825);
#7342=VERTEX_POINT('',#31968);
#7343=VERTEX_POINT('',#32041);
#7344=VERTEX_POINT('',#32184);
#7345=VERTEX_POINT('',#32257);
#7346=VERTEX_POINT('',#32400);
#7347=VERTEX_POINT('',#32473);
#7348=VERTEX_POINT('',#32616);
#7349=VERTEX_POINT('',#32689);
#7350=VERTEX_POINT('',#32832);
#7351=VERTEX_POINT('',#32905);
#7352=VERTEX_POINT('',#33048);
#7353=VERTEX_POINT('',#33121);
#7354=VERTEX_POINT('',#33264);
#7355=VERTEX_POINT('',#33337);
#7356=VERTEX_POINT('',#33480);
#7357=VERTEX_POINT('',#33553);
#7358=VERTEX_POINT('',#33696);
#7359=VERTEX_POINT('',#33769);
#7360=VERTEX_POINT('',#33912);
#7361=VERTEX_POINT('',#33985);
#7362=VERTEX_POINT('',#34128);
#7363=VERTEX_POINT('',#34201);
#7364=VERTEX_POINT('',#34344);
#7365=VERTEX_POINT('',#34421);
#7366=VERTEX_POINT('',#34424);
#7367=VERTEX_POINT('',#34428);
#7368=VERTEX_POINT('',#34432);
#7369=VERTEX_POINT('',#34436);
#7370=VERTEX_POINT('',#34439);
#7371=VERTEX_POINT('',#34443);
#7372=VERTEX_POINT('',#34447);
#7373=VERTEX_POINT('',#34452);
#7374=VERTEX_POINT('',#34453);
#7375=VERTEX_POINT('',#34455);
#7376=VERTEX_POINT('',#34457);
#7377=VERTEX_POINT('',#34461);
#7378=VERTEX_POINT('',#34463);
#7379=VERTEX_POINT('',#34467);
#7380=VERTEX_POINT('',#34469);
#7381=VERTEX_POINT('',#34473);
#7382=VERTEX_POINT('',#34475);
#7383=VERTEX_POINT('',#34479);
#7384=VERTEX_POINT('',#34481);
#7385=VERTEX_POINT('',#34573);
#7386=VERTEX_POINT('',#34574);
#7387=VERTEX_POINT('',#34576);
#7388=VERTEX_POINT('',#34578);
#7389=VERTEX_POINT('',#34580);
#7390=VERTEX_POINT('',#34582);
#7391=VERTEX_POINT('',#34584);
#7392=VERTEX_POINT('',#34586);
#7393=VERTEX_POINT('',#34590);
#7394=VERTEX_POINT('',#34592);
#7395=VERTEX_POINT('',#34596);
#7396=VERTEX_POINT('',#34600);
#7397=VERTEX_POINT('',#34604);
#7398=VERTEX_POINT('',#34608);
#7399=VERTEX_POINT('',#34610);
#7400=VERTEX_POINT('',#34612);
#7401=VERTEX_POINT('',#34624);
#7402=VERTEX_POINT('',#34626);
#7403=VERTEX_POINT('',#34630);
#7404=VERTEX_POINT('',#34632);
#7405=VERTEX_POINT('',#34639);
#7406=VERTEX_POINT('',#34642);
#7407=VERTEX_POINT('',#34646);
#7408=VERTEX_POINT('',#34650);
#7409=VERTEX_POINT('',#34654);
#7410=VERTEX_POINT('',#34657);
#7411=VERTEX_POINT('',#34661);
#7412=VERTEX_POINT('',#34665);
#7413=VERTEX_POINT('',#34670);
#7414=VERTEX_POINT('',#34671);
#7415=VERTEX_POINT('',#34673);
#7416=VERTEX_POINT('',#34675);
#7417=VERTEX_POINT('',#34679);
#7418=VERTEX_POINT('',#34681);
#7419=VERTEX_POINT('',#34685);
#7420=VERTEX_POINT('',#34687);
#7421=VERTEX_POINT('',#34691);
#7422=VERTEX_POINT('',#34693);
#7423=VERTEX_POINT('',#34697);
#7424=VERTEX_POINT('',#34699);
#7425=VERTEX_POINT('',#34726);
#7426=VERTEX_POINT('',#34728);
#7427=VERTEX_POINT('',#34732);
#7428=VERTEX_POINT('',#34734);
#7429=EDGE_CURVE('',#6224,#6224,#5806,.T.);
#7430=EDGE_CURVE('',#6224,#6225,#3224,.T.);
#7431=EDGE_CURVE('',#6225,#6225,#5807,.T.);
#7432=EDGE_CURVE('',#6226,#6226,#5808,.T.);
#7433=EDGE_CURVE('',#6226,#6227,#3225,.T.);
#7434=EDGE_CURVE('',#6227,#6227,#5809,.T.);
#7435=EDGE_CURVE('',#6228,#6228,#5810,.T.);
#7436=EDGE_CURVE('',#6228,#6229,#3226,.T.);
#7437=EDGE_CURVE('',#6229,#6229,#5811,.T.);
#7438=EDGE_CURVE('',#6230,#6230,#5812,.T.);
#7439=EDGE_CURVE('',#6230,#6231,#3227,.T.);
#7440=EDGE_CURVE('',#6231,#6231,#5813,.T.);
#7441=EDGE_CURVE('',#6232,#6233,#3228,.T.);
#7442=EDGE_CURVE('',#6233,#6234,#3229,.T.);
#7443=EDGE_CURVE('',#6235,#6234,#3230,.T.);
#7444=EDGE_CURVE('',#6232,#6235,#3231,.T.);
#7445=EDGE_CURVE('',#6236,#6232,#3232,.T.);
#7446=EDGE_CURVE('',#6237,#6235,#3233,.T.);
#7447=EDGE_CURVE('',#6236,#6237,#3234,.T.);
#7448=EDGE_CURVE('',#6238,#6236,#3235,.T.);
#7449=EDGE_CURVE('',#6239,#6237,#3236,.T.);
#7450=EDGE_CURVE('',#6238,#6239,#3237,.T.);
#7451=EDGE_CURVE('',#6233,#6238,#3238,.T.);
#7452=EDGE_CURVE('',#6234,#6239,#3239,.T.);
#7453=EDGE_CURVE('',#6240,#6241,#3240,.T.);
#7454=EDGE_CURVE('',#6241,#6242,#3241,.T.);
#7455=EDGE_CURVE('',#6243,#6242,#3242,.T.);
#7456=EDGE_CURVE('',#6240,#6243,#3243,.T.);
#7457=EDGE_CURVE('',#6244,#6240,#3244,.T.);
#7458=EDGE_CURVE('',#6245,#6243,#3245,.T.);
#7459=EDGE_CURVE('',#6244,#6245,#3246,.T.);
#7460=EDGE_CURVE('',#6246,#6244,#3247,.T.);
#7461=EDGE_CURVE('',#6247,#6245,#3248,.T.);
#7462=EDGE_CURVE('',#6246,#6247,#3249,.T.);
#7463=EDGE_CURVE('',#6241,#6246,#3250,.T.);
#7464=EDGE_CURVE('',#6242,#6247,#3251,.T.);
#7465=EDGE_CURVE('',#6248,#6249,#3252,.T.);
#7466=EDGE_CURVE('',#6249,#6250,#3253,.T.);
#7467=EDGE_CURVE('',#6251,#6250,#3254,.T.);
#7468=EDGE_CURVE('',#6248,#6251,#3255,.T.);
#7469=EDGE_CURVE('',#6252,#6248,#3256,.T.);
#7470=EDGE_CURVE('',#6253,#6251,#3257,.T.);
#7471=EDGE_CURVE('',#6252,#6253,#3258,.T.);
#7472=EDGE_CURVE('',#6254,#6252,#3259,.T.);
#7473=EDGE_CURVE('',#6255,#6253,#3260,.T.);
#7474=EDGE_CURVE('',#6254,#6255,#3261,.T.);
#7475=EDGE_CURVE('',#6249,#6254,#3262,.T.);
#7476=EDGE_CURVE('',#6250,#6255,#3263,.T.);
#7477=EDGE_CURVE('',#6256,#6256,#5814,.T.);
#7478=EDGE_CURVE('',#6256,#6257,#3264,.T.);
#7479=EDGE_CURVE('',#6257,#6257,#5815,.T.);
#7480=EDGE_CURVE('',#6258,#6258,#5816,.T.);
#7481=EDGE_CURVE('',#6258,#6259,#3265,.T.);
#7482=EDGE_CURVE('',#6259,#6259,#5817,.T.);
#7483=EDGE_CURVE('',#6260,#6260,#5818,.T.);
#7484=EDGE_CURVE('',#6260,#6261,#3266,.T.);
#7485=EDGE_CURVE('',#6261,#6261,#5819,.T.);
#7486=EDGE_CURVE('',#6262,#6262,#5820,.T.);
#7487=EDGE_CURVE('',#6262,#6263,#3267,.T.);
#7488=EDGE_CURVE('',#6263,#6263,#5821,.T.);
#7489=EDGE_CURVE('',#6264,#6264,#5822,.T.);
#7490=EDGE_CURVE('',#6264,#6265,#3268,.T.);
#7491=EDGE_CURVE('',#6265,#6265,#5823,.T.);
#7492=EDGE_CURVE('',#6266,#6266,#5824,.T.);
#7493=EDGE_CURVE('',#6266,#6267,#3269,.T.);
#7494=EDGE_CURVE('',#6267,#6267,#5825,.T.);
#7495=EDGE_CURVE('',#6268,#6268,#5826,.T.);
#7496=EDGE_CURVE('',#6268,#6269,#3270,.T.);
#7497=EDGE_CURVE('',#6269,#6269,#5827,.T.);
#7498=EDGE_CURVE('',#6270,#6270,#5828,.T.);
#7499=EDGE_CURVE('',#6270,#6271,#3271,.T.);
#7500=EDGE_CURVE('',#6271,#6271,#5829,.T.);
#7501=EDGE_CURVE('',#6272,#6272,#5830,.T.);
#7502=EDGE_CURVE('',#6272,#6273,#3272,.T.);
#7503=EDGE_CURVE('',#6273,#6273,#5831,.T.);
#7504=EDGE_CURVE('',#6274,#6274,#5832,.T.);
#7505=EDGE_CURVE('',#6274,#6275,#3273,.T.);
#7506=EDGE_CURVE('',#6275,#6275,#5833,.T.);
#7507=EDGE_CURVE('',#6276,#6276,#5834,.T.);
#7508=EDGE_CURVE('',#6276,#6277,#3274,.T.);
#7509=EDGE_CURVE('',#6277,#6277,#5835,.T.);
#7510=EDGE_CURVE('',#6278,#6278,#5836,.T.);
#7511=EDGE_CURVE('',#6278,#6279,#3275,.T.);
#7512=EDGE_CURVE('',#6279,#6279,#5837,.T.);
#7513=EDGE_CURVE('',#6280,#6280,#5838,.T.);
#7514=EDGE_CURVE('',#6280,#6281,#3276,.T.);
#7515=EDGE_CURVE('',#6281,#6281,#5839,.T.);
#7516=EDGE_CURVE('',#6282,#6282,#5840,.T.);
#7517=EDGE_CURVE('',#6282,#6283,#3277,.T.);
#7518=EDGE_CURVE('',#6283,#6283,#5841,.T.);
#7519=EDGE_CURVE('',#6284,#6284,#5842,.T.);
#7520=EDGE_CURVE('',#6284,#6285,#3278,.T.);
#7521=EDGE_CURVE('',#6285,#6285,#5843,.T.);
#7522=EDGE_CURVE('',#6286,#6286,#5844,.T.);
#7523=EDGE_CURVE('',#6286,#6287,#3279,.T.);
#7524=EDGE_CURVE('',#6287,#6287,#5845,.T.);
#7525=EDGE_CURVE('',#6288,#6289,#3280,.T.);
#7526=EDGE_CURVE('',#6289,#6290,#3281,.T.);
#7527=EDGE_CURVE('',#6291,#6290,#3282,.T.);
#7528=EDGE_CURVE('',#6288,#6291,#3283,.T.);
#7529=EDGE_CURVE('',#6292,#6288,#3284,.T.);
#7530=EDGE_CURVE('',#6293,#6291,#3285,.T.);
#7531=EDGE_CURVE('',#6292,#6293,#3286,.T.);
#7532=EDGE_CURVE('',#6294,#6292,#3287,.T.);
#7533=EDGE_CURVE('',#6295,#6293,#3288,.T.);
#7534=EDGE_CURVE('',#6294,#6295,#3289,.T.);
#7535=EDGE_CURVE('',#6289,#6294,#3290,.T.);
#7536=EDGE_CURVE('',#6290,#6295,#3291,.T.);
#7537=EDGE_CURVE('',#6296,#6296,#5846,.T.);
#7538=EDGE_CURVE('',#6296,#6297,#3292,.T.);
#7539=EDGE_CURVE('',#6297,#6297,#5847,.T.);
#7540=EDGE_CURVE('',#6298,#6298,#5848,.T.);
#7541=EDGE_CURVE('',#6299,#6299,#5849,.T.);
#7542=EDGE_CURVE('',#6299,#6300,#3293,.T.);
#7543=EDGE_CURVE('',#6300,#6300,#5850,.T.);
#7544=EDGE_CURVE('',#6301,#6301,#5851,.T.);
#7545=EDGE_CURVE('',#6302,#6302,#5852,.T.);
#7546=EDGE_CURVE('',#6302,#6298,#3294,.T.);
#7547=EDGE_CURVE('',#6303,#6303,#5853,.T.);
#7548=EDGE_CURVE('',#6303,#6301,#3295,.T.);
#7549=EDGE_CURVE('',#6304,#6305,#3296,.T.);
#7550=EDGE_CURVE('',#6305,#6306,#3297,.T.);
#7551=EDGE_CURVE('',#6307,#6306,#3298,.T.);
#7552=EDGE_CURVE('',#6304,#6307,#3299,.T.);
#7553=EDGE_CURVE('',#6308,#6304,#3300,.T.);
#7554=EDGE_CURVE('',#6309,#6307,#3301,.T.);
#7555=EDGE_CURVE('',#6308,#6309,#3302,.T.);
#7556=EDGE_CURVE('',#6310,#6308,#3303,.T.);
#7557=EDGE_CURVE('',#6311,#6309,#3304,.T.);
#7558=EDGE_CURVE('',#6310,#6311,#3305,.T.);
#7559=EDGE_CURVE('',#6305,#6310,#3306,.T.);
#7560=EDGE_CURVE('',#6306,#6311,#3307,.T.);
#7561=EDGE_CURVE('',#6312,#6313,#3308,.T.);
#7562=EDGE_CURVE('',#6313,#6314,#3309,.T.);
#7563=EDGE_CURVE('',#6315,#6314,#3310,.T.);
#7564=EDGE_CURVE('',#6312,#6315,#3311,.T.);
#7565=EDGE_CURVE('',#6316,#6312,#3312,.T.);
#7566=EDGE_CURVE('',#6317,#6315,#3313,.T.);
#7567=EDGE_CURVE('',#6316,#6317,#3314,.T.);
#7568=EDGE_CURVE('',#6318,#6316,#3315,.T.);
#7569=EDGE_CURVE('',#6319,#6317,#3316,.T.);
#7570=EDGE_CURVE('',#6318,#6319,#3317,.T.);
#7571=EDGE_CURVE('',#6313,#6318,#3318,.T.);
#7572=EDGE_CURVE('',#6314,#6319,#3319,.T.);
#7573=EDGE_CURVE('',#6320,#6320,#5854,.T.);
#7574=EDGE_CURVE('',#6320,#6321,#3320,.T.);
#7575=EDGE_CURVE('',#6321,#6321,#5855,.T.);
#7576=EDGE_CURVE('',#6322,#6322,#5856,.T.);
#7577=EDGE_CURVE('',#6323,#6323,#5857,.T.);
#7578=EDGE_CURVE('',#6323,#6324,#3321,.T.);
#7579=EDGE_CURVE('',#6324,#6324,#5858,.T.);
#7580=EDGE_CURVE('',#6325,#6325,#5859,.T.);
#7581=EDGE_CURVE('',#6326,#6326,#5860,.T.);
#7582=EDGE_CURVE('',#6326,#6322,#3322,.T.);
#7583=EDGE_CURVE('',#6327,#6327,#5861,.T.);
#7584=EDGE_CURVE('',#6327,#6325,#3323,.T.);
#7585=EDGE_CURVE('',#6328,#6329,#3324,.T.);
#7586=EDGE_CURVE('',#6329,#6330,#3325,.T.);
#7587=EDGE_CURVE('',#6331,#6330,#3326,.T.);
#7588=EDGE_CURVE('',#6328,#6331,#3327,.T.);
#7589=EDGE_CURVE('',#6332,#6328,#3328,.T.);
#7590=EDGE_CURVE('',#6333,#6331,#3329,.T.);
#7591=EDGE_CURVE('',#6332,#6333,#3330,.T.);
#7592=EDGE_CURVE('',#6334,#6332,#3331,.T.);
#7593=EDGE_CURVE('',#6335,#6333,#3332,.T.);
#7594=EDGE_CURVE('',#6334,#6335,#3333,.T.);
#7595=EDGE_CURVE('',#6329,#6334,#3334,.T.);
#7596=EDGE_CURVE('',#6330,#6335,#3335,.T.);
#7597=EDGE_CURVE('',#6336,#6337,#3336,.T.);
#7598=EDGE_CURVE('',#6337,#6338,#3337,.T.);
#7599=EDGE_CURVE('',#6339,#6338,#3338,.T.);
#7600=EDGE_CURVE('',#6336,#6339,#3339,.T.);
#7601=EDGE_CURVE('',#6340,#6336,#3340,.T.);
#7602=EDGE_CURVE('',#6341,#6339,#3341,.T.);
#7603=EDGE_CURVE('',#6340,#6341,#3342,.T.);
#7604=EDGE_CURVE('',#6342,#6340,#3343,.T.);
#7605=EDGE_CURVE('',#6343,#6341,#3344,.T.);
#7606=EDGE_CURVE('',#6342,#6343,#3345,.T.);
#7607=EDGE_CURVE('',#6337,#6342,#3346,.T.);
#7608=EDGE_CURVE('',#6338,#6343,#3347,.T.);
#7609=EDGE_CURVE('',#6344,#6344,#5862,.T.);
#7610=EDGE_CURVE('',#6344,#6345,#3348,.T.);
#7611=EDGE_CURVE('',#6345,#6345,#5863,.T.);
#7612=EDGE_CURVE('',#6346,#6346,#5864,.T.);
#7613=EDGE_CURVE('',#6346,#6347,#3349,.T.);
#7614=EDGE_CURVE('',#6347,#6347,#5865,.T.);
#7615=EDGE_CURVE('',#6348,#6348,#5866,.T.);
#7616=EDGE_CURVE('',#6348,#6349,#3350,.T.);
#7617=EDGE_CURVE('',#6349,#6349,#5867,.T.);
#7618=EDGE_CURVE('',#6350,#6350,#5868,.T.);
#7619=EDGE_CURVE('',#6350,#6351,#3351,.T.);
#7620=EDGE_CURVE('',#6351,#6351,#5869,.T.);
#7621=EDGE_CURVE('',#6352,#6352,#5870,.T.);
#7622=EDGE_CURVE('',#6352,#6353,#3352,.T.);
#7623=EDGE_CURVE('',#6353,#6353,#5871,.T.);
#7624=EDGE_CURVE('',#6354,#6354,#5872,.T.);
#7625=EDGE_CURVE('',#6354,#6355,#3353,.T.);
#7626=EDGE_CURVE('',#6355,#6355,#5873,.T.);
#7627=EDGE_CURVE('',#6356,#6356,#5874,.T.);
#7628=EDGE_CURVE('',#6356,#6357,#3354,.T.);
#7629=EDGE_CURVE('',#6357,#6357,#5875,.T.);
#7630=EDGE_CURVE('',#6358,#6359,#3355,.T.);
#7631=EDGE_CURVE('',#6360,#6358,#3356,.T.);
#7632=EDGE_CURVE('',#6360,#6361,#3357,.T.);
#7633=EDGE_CURVE('',#6359,#6361,#3358,.T.);
#7634=EDGE_CURVE('',#6362,#6363,#3359,.T.);
#7635=EDGE_CURVE('',#6364,#6362,#3360,.T.);
#7636=EDGE_CURVE('',#6365,#6364,#3361,.T.);
#7637=EDGE_CURVE('',#6363,#6365,#3362,.T.);
#7638=EDGE_CURVE('',#6365,#6366,#3363,.T.);
#7639=EDGE_CURVE('',#6367,#6364,#3364,.T.);
#7640=EDGE_CURVE('',#6366,#6367,#3365,.T.);
#7641=EDGE_CURVE('',#6368,#6360,#3366,.T.);
#7642=EDGE_CURVE('',#6368,#6369,#3367,.T.);
#7643=EDGE_CURVE('',#6361,#6369,#3368,.T.);
#7644=EDGE_CURVE('',#6358,#6370,#3369,.T.);
#7645=EDGE_CURVE('',#6371,#6370,#3370,.T.);
#7646=EDGE_CURVE('',#6363,#6371,#3371,.T.);
#7647=EDGE_CURVE('',#6366,#6368,#3372,.T.);
#7648=EDGE_CURVE('',#6359,#6372,#3373,.T.);
#7649=EDGE_CURVE('',#6370,#6372,#3374,.T.);
#7650=EDGE_CURVE('',#6362,#6373,#3375,.T.);
#7651=EDGE_CURVE('',#6372,#6373,#3376,.T.);
#7652=EDGE_CURVE('',#6369,#6367,#3377,.T.);
#7653=EDGE_CURVE('',#6373,#6371,#3378,.T.);
#7654=EDGE_CURVE('',#6374,#6374,#5876,.T.);
#7655=EDGE_CURVE('',#6374,#6375,#3379,.T.);
#7656=EDGE_CURVE('',#6375,#6375,#5877,.T.);
#7657=EDGE_CURVE('',#6376,#6376,#5878,.T.);
#7658=EDGE_CURVE('',#6376,#6377,#3380,.T.);
#7659=EDGE_CURVE('',#6377,#6377,#5879,.T.);
#7660=EDGE_CURVE('',#6378,#6378,#5880,.T.);
#7661=EDGE_CURVE('',#6378,#6379,#3381,.T.);
#7662=EDGE_CURVE('',#6379,#6379,#5881,.T.);
#7663=EDGE_CURVE('',#6380,#6380,#5882,.T.);
#7664=EDGE_CURVE('',#6380,#6381,#3382,.T.);
#7665=EDGE_CURVE('',#6381,#6381,#5883,.T.);
#7666=EDGE_CURVE('',#6382,#6382,#5884,.T.);
#7667=EDGE_CURVE('',#6382,#6383,#3383,.T.);
#7668=EDGE_CURVE('',#6383,#6383,#5885,.T.);
#7669=EDGE_CURVE('',#6384,#6384,#5886,.T.);
#7670=EDGE_CURVE('',#6384,#6385,#3384,.T.);
#7671=EDGE_CURVE('',#6385,#6385,#5887,.T.);
#7672=EDGE_CURVE('',#6386,#6386,#5888,.T.);
#7673=EDGE_CURVE('',#6386,#6387,#3385,.T.);
#7674=EDGE_CURVE('',#6387,#6387,#5889,.T.);
#7675=EDGE_CURVE('',#6388,#6388,#5890,.T.);
#7676=EDGE_CURVE('',#6388,#6389,#3386,.T.);
#7677=EDGE_CURVE('',#6389,#6389,#5891,.T.);
#7678=EDGE_CURVE('',#6390,#6390,#5892,.T.);
#7679=EDGE_CURVE('',#6390,#6391,#3387,.T.);
#7680=EDGE_CURVE('',#6391,#6391,#5893,.T.);
#7681=EDGE_CURVE('',#6392,#6392,#5894,.T.);
#7682=EDGE_CURVE('',#6392,#6393,#3388,.T.);
#7683=EDGE_CURVE('',#6393,#6393,#5895,.T.);
#7684=EDGE_CURVE('',#6394,#6394,#5896,.T.);
#7685=EDGE_CURVE('',#6394,#6395,#3389,.T.);
#7686=EDGE_CURVE('',#6395,#6395,#5897,.T.);
#7687=EDGE_CURVE('',#6396,#6396,#5898,.T.);
#7688=EDGE_CURVE('',#6396,#6397,#3390,.T.);
#7689=EDGE_CURVE('',#6397,#6397,#5899,.T.);
#7690=EDGE_CURVE('',#6398,#6398,#5900,.T.);
#7691=EDGE_CURVE('',#6399,#6399,#5901,.T.);
#7692=EDGE_CURVE('',#6399,#6398,#3391,.T.);
#7693=EDGE_CURVE('',#6400,#6400,#5902,.T.);
#7694=EDGE_CURVE('',#6400,#6401,#3392,.T.);
#7695=EDGE_CURVE('',#6401,#6401,#5903,.T.);
#7696=EDGE_CURVE('',#6402,#6402,#5904,.T.);
#7697=EDGE_CURVE('',#6402,#6403,#3393,.T.);
#7698=EDGE_CURVE('',#6403,#6403,#5905,.T.);
#7699=EDGE_CURVE('',#6404,#6404,#5906,.T.);
#7700=EDGE_CURVE('',#6404,#6405,#3394,.T.);
#7701=EDGE_CURVE('',#6405,#6405,#5907,.T.);
#7702=EDGE_CURVE('',#6406,#6406,#5908,.T.);
#7703=EDGE_CURVE('',#6406,#6407,#3395,.T.);
#7704=EDGE_CURVE('',#6407,#6407,#5909,.T.);
#7705=EDGE_CURVE('',#6408,#6408,#5910,.T.);
#7706=EDGE_CURVE('',#6408,#6409,#3396,.T.);
#7707=EDGE_CURVE('',#6409,#6409,#5911,.T.);
#7708=EDGE_CURVE('',#6410,#6410,#5912,.T.);
#7709=EDGE_CURVE('',#6410,#6411,#3397,.T.);
#7710=EDGE_CURVE('',#6411,#6411,#5913,.T.);
#7711=EDGE_CURVE('',#6412,#6412,#5914,.T.);
#7712=EDGE_CURVE('',#6412,#6413,#3398,.T.);
#7713=EDGE_CURVE('',#6413,#6413,#5915,.T.);
#7714=EDGE_CURVE('',#6414,#6414,#5916,.T.);
#7715=EDGE_CURVE('',#6414,#6415,#3399,.T.);
#7716=EDGE_CURVE('',#6415,#6415,#5917,.T.);
#7717=EDGE_CURVE('',#6416,#6417,#3400,.T.);
#7718=EDGE_CURVE('',#6418,#6416,#3401,.T.);
#7719=EDGE_CURVE('',#6418,#6419,#3402,.T.);
#7720=EDGE_CURVE('',#6417,#6419,#3403,.T.);
#7721=EDGE_CURVE('',#6420,#6421,#3404,.T.);
#7722=EDGE_CURVE('',#6422,#6420,#3405,.T.);
#7723=EDGE_CURVE('',#6423,#6422,#3406,.T.);
#7724=EDGE_CURVE('',#6421,#6423,#3407,.T.);
#7725=EDGE_CURVE('',#6423,#6424,#3408,.T.);
#7726=EDGE_CURVE('',#6425,#6422,#3409,.T.);
#7727=EDGE_CURVE('',#6424,#6425,#3410,.T.);
#7728=EDGE_CURVE('',#6426,#6418,#3411,.T.);
#7729=EDGE_CURVE('',#6426,#6427,#3412,.T.);
#7730=EDGE_CURVE('',#6419,#6427,#3413,.T.);
#7731=EDGE_CURVE('',#6416,#6428,#3414,.T.);
#7732=EDGE_CURVE('',#6429,#6428,#3415,.T.);
#7733=EDGE_CURVE('',#6421,#6429,#3416,.T.);
#7734=EDGE_CURVE('',#6424,#6426,#3417,.T.);
#7735=EDGE_CURVE('',#6417,#6430,#3418,.T.);
#7736=EDGE_CURVE('',#6428,#6430,#3419,.T.);
#7737=EDGE_CURVE('',#6420,#6431,#3420,.T.);
#7738=EDGE_CURVE('',#6430,#6431,#3421,.T.);
#7739=EDGE_CURVE('',#6427,#6425,#3422,.T.);
#7740=EDGE_CURVE('',#6431,#6429,#3423,.T.);
#7741=EDGE_CURVE('',#6432,#6432,#5918,.T.);
#7742=EDGE_CURVE('',#6432,#6433,#3424,.T.);
#7743=EDGE_CURVE('',#6433,#6433,#5919,.T.);
#7744=EDGE_CURVE('',#6434,#6434,#5920,.T.);
#7745=EDGE_CURVE('',#6434,#6435,#3425,.T.);
#7746=EDGE_CURVE('',#6435,#6435,#5921,.T.);
#7747=EDGE_CURVE('',#6436,#6436,#5922,.T.);
#7748=EDGE_CURVE('',#6436,#6437,#3426,.T.);
#7749=EDGE_CURVE('',#6437,#6437,#5923,.T.);
#7750=EDGE_CURVE('',#6438,#6438,#5924,.T.);
#7751=EDGE_CURVE('',#6438,#6439,#3427,.T.);
#7752=EDGE_CURVE('',#6439,#6439,#5925,.T.);
#7753=EDGE_CURVE('',#6440,#6440,#5926,.T.);
#7754=EDGE_CURVE('',#6440,#6441,#3428,.T.);
#7755=EDGE_CURVE('',#6441,#6441,#5927,.T.);
#7756=EDGE_CURVE('',#6442,#6442,#5928,.T.);
#7757=EDGE_CURVE('',#6442,#6443,#3429,.T.);
#7758=EDGE_CURVE('',#6443,#6443,#5929,.T.);
#7759=EDGE_CURVE('',#6444,#6444,#5930,.T.);
#7760=EDGE_CURVE('',#6444,#6445,#3430,.T.);
#7761=EDGE_CURVE('',#6445,#6445,#5931,.T.);
#7762=EDGE_CURVE('',#6446,#6446,#5932,.T.);
#7763=EDGE_CURVE('',#6446,#6447,#3431,.T.);
#7764=EDGE_CURVE('',#6447,#6447,#5933,.T.);
#7765=EDGE_CURVE('',#6448,#6448,#5934,.T.);
#7766=EDGE_CURVE('',#6448,#6449,#3432,.T.);
#7767=EDGE_CURVE('',#6449,#6449,#5935,.T.);
#7768=EDGE_CURVE('',#6450,#6450,#5936,.T.);
#7769=EDGE_CURVE('',#6450,#6451,#3433,.T.);
#7770=EDGE_CURVE('',#6451,#6451,#5937,.T.);
#7771=EDGE_CURVE('',#6452,#6452,#5938,.T.);
#7772=EDGE_CURVE('',#6452,#6453,#3434,.T.);
#7773=EDGE_CURVE('',#6453,#6453,#5939,.T.);
#7774=EDGE_CURVE('',#6454,#6454,#5940,.T.);
#7775=EDGE_CURVE('',#6454,#6455,#3435,.T.);
#7776=EDGE_CURVE('',#6455,#6455,#5941,.T.);
#7777=EDGE_CURVE('',#6456,#6456,#5942,.T.);
#7778=EDGE_CURVE('',#6457,#6457,#5943,.T.);
#7779=EDGE_CURVE('',#6457,#6456,#3436,.T.);
#7780=EDGE_CURVE('',#6458,#6458,#5944,.T.);
#7781=EDGE_CURVE('',#6458,#6459,#3437,.T.);
#7782=EDGE_CURVE('',#6459,#6459,#5945,.T.);
#7783=EDGE_CURVE('',#6460,#6461,#3438,.T.);
#7784=EDGE_CURVE('',#6460,#6462,#3439,.T.);
#7785=EDGE_CURVE('',#6463,#6462,#3440,.T.);
#7786=EDGE_CURVE('',#6461,#6463,#3441,.T.);
#7787=EDGE_CURVE('',#6464,#6460,#3442,.T.);
#7788=EDGE_CURVE('',#6464,#6465,#3443,.T.);
#7789=EDGE_CURVE('',#6462,#6465,#3444,.T.);
#7790=EDGE_CURVE('',#6466,#6464,#3445,.T.);
#7791=EDGE_CURVE('',#6466,#6467,#3446,.T.);
#7792=EDGE_CURVE('',#6465,#6467,#3447,.T.);
#7793=EDGE_CURVE('',#6468,#6466,#3448,.T.);
#7794=EDGE_CURVE('',#6468,#6469,#3449,.T.);
#7795=EDGE_CURVE('',#6467,#6469,#3450,.T.);
#7796=EDGE_CURVE('',#6470,#6468,#3451,.T.);
#7797=EDGE_CURVE('',#6470,#6471,#3452,.T.);
#7798=EDGE_CURVE('',#6469,#6471,#3453,.T.);
#7799=EDGE_CURVE('',#6472,#6470,#3454,.T.);
#7800=EDGE_CURVE('',#6472,#6473,#3455,.T.);
#7801=EDGE_CURVE('',#6471,#6473,#3456,.T.);
#7802=EDGE_CURVE('',#6474,#6472,#3457,.T.);
#7803=EDGE_CURVE('',#6474,#6475,#3458,.T.);
#7804=EDGE_CURVE('',#6473,#6475,#3459,.T.);
#7805=EDGE_CURVE('',#6476,#6474,#3460,.T.);
#7806=EDGE_CURVE('',#6476,#6477,#3461,.T.);
#7807=EDGE_CURVE('',#6475,#6477,#3462,.T.);
#7808=EDGE_CURVE('',#6478,#6476,#3463,.T.);
#7809=EDGE_CURVE('',#6479,#6478,#3464,.T.);
#7810=EDGE_CURVE('',#6477,#6479,#3465,.T.);
#7811=EDGE_CURVE('',#6480,#6481,#3466,.T.);
#7812=EDGE_CURVE('',#6480,#6482,#3467,.T.);
#7813=EDGE_CURVE('',#6483,#6482,#3468,.T.);
#7814=EDGE_CURVE('',#6481,#6483,#3469,.T.);
#7815=EDGE_CURVE('',#6484,#6480,#3470,.T.);
#7816=EDGE_CURVE('',#6484,#6485,#3471,.T.);
#7817=EDGE_CURVE('',#6482,#6485,#3472,.T.);
#7818=EDGE_CURVE('',#6486,#6484,#3473,.T.);
#7819=EDGE_CURVE('',#6486,#6487,#3474,.T.);
#7820=EDGE_CURVE('',#6485,#6487,#3475,.T.);
#7821=EDGE_CURVE('',#6488,#6486,#3476,.T.);
#7822=EDGE_CURVE('',#6488,#6489,#3477,.T.);
#7823=EDGE_CURVE('',#6487,#6489,#3478,.T.);
#7824=EDGE_CURVE('',#6490,#6488,#3479,.T.);
#7825=EDGE_CURVE('',#6490,#6491,#3480,.T.);
#7826=EDGE_CURVE('',#6489,#6491,#3481,.T.);
#7827=EDGE_CURVE('',#6492,#6490,#3482,.T.);
#7828=EDGE_CURVE('',#6492,#6493,#3483,.T.);
#7829=EDGE_CURVE('',#6491,#6493,#3484,.T.);
#7830=EDGE_CURVE('',#6494,#6492,#3485,.T.);
#7831=EDGE_CURVE('',#6494,#6495,#3486,.T.);
#7832=EDGE_CURVE('',#6493,#6495,#3487,.T.);
#7833=EDGE_CURVE('',#6496,#6494,#3488,.T.);
#7834=EDGE_CURVE('',#6496,#6497,#3489,.T.);
#7835=EDGE_CURVE('',#6495,#6497,#3490,.T.);
#7836=EDGE_CURVE('',#6498,#6496,#3491,.T.);
#7837=EDGE_CURVE('',#6499,#6498,#3492,.T.);
#7838=EDGE_CURVE('',#6497,#6499,#3493,.T.);
#7839=EDGE_CURVE('',#6500,#6501,#3494,.T.);
#7840=EDGE_CURVE('',#6500,#6502,#3495,.T.);
#7841=EDGE_CURVE('',#6503,#6502,#3496,.T.);
#7842=EDGE_CURVE('',#6501,#6503,#3497,.T.);
#7843=EDGE_CURVE('',#6504,#6500,#3498,.T.);
#7844=EDGE_CURVE('',#6504,#6505,#3499,.T.);
#7845=EDGE_CURVE('',#6502,#6505,#3500,.T.);
#7846=EDGE_CURVE('',#6506,#6504,#3501,.T.);
#7847=EDGE_CURVE('',#6506,#6507,#3502,.T.);
#7848=EDGE_CURVE('',#6505,#6507,#3503,.T.);
#7849=EDGE_CURVE('',#6508,#6506,#3504,.T.);
#7850=EDGE_CURVE('',#6508,#6509,#3505,.T.);
#7851=EDGE_CURVE('',#6507,#6509,#3506,.T.);
#7852=EDGE_CURVE('',#6510,#6508,#3507,.T.);
#7853=EDGE_CURVE('',#6510,#6511,#3508,.T.);
#7854=EDGE_CURVE('',#6509,#6511,#3509,.T.);
#7855=EDGE_CURVE('',#6512,#6510,#3510,.T.);
#7856=EDGE_CURVE('',#6512,#6513,#3511,.T.);
#7857=EDGE_CURVE('',#6511,#6513,#3512,.T.);
#7858=EDGE_CURVE('',#6514,#6512,#3513,.T.);
#7859=EDGE_CURVE('',#6514,#6515,#3514,.T.);
#7860=EDGE_CURVE('',#6513,#6515,#3515,.T.);
#7861=EDGE_CURVE('',#6516,#6514,#3516,.T.);
#7862=EDGE_CURVE('',#6516,#6517,#3517,.T.);
#7863=EDGE_CURVE('',#6515,#6517,#3518,.T.);
#7864=EDGE_CURVE('',#6518,#6516,#3519,.T.);
#7865=EDGE_CURVE('',#6519,#6518,#3520,.T.);
#7866=EDGE_CURVE('',#6517,#6519,#3521,.T.);
#7867=EDGE_CURVE('',#6520,#6521,#3522,.T.);
#7868=EDGE_CURVE('',#6520,#6522,#3523,.T.);
#7869=EDGE_CURVE('',#6523,#6522,#3524,.T.);
#7870=EDGE_CURVE('',#6521,#6523,#3525,.T.);
#7871=EDGE_CURVE('',#6524,#6520,#3526,.T.);
#7872=EDGE_CURVE('',#6524,#6525,#3527,.T.);
#7873=EDGE_CURVE('',#6522,#6525,#3528,.T.);
#7874=EDGE_CURVE('',#6526,#6524,#3529,.T.);
#7875=EDGE_CURVE('',#6526,#6527,#3530,.T.);
#7876=EDGE_CURVE('',#6525,#6527,#3531,.T.);
#7877=EDGE_CURVE('',#6528,#6526,#3532,.T.);
#7878=EDGE_CURVE('',#6528,#6529,#3533,.T.);
#7879=EDGE_CURVE('',#6527,#6529,#3534,.T.);
#7880=EDGE_CURVE('',#6530,#6528,#3535,.T.);
#7881=EDGE_CURVE('',#6530,#6531,#3536,.T.);
#7882=EDGE_CURVE('',#6529,#6531,#3537,.T.);
#7883=EDGE_CURVE('',#6532,#6530,#3538,.T.);
#7884=EDGE_CURVE('',#6532,#6533,#3539,.T.);
#7885=EDGE_CURVE('',#6531,#6533,#3540,.T.);
#7886=EDGE_CURVE('',#6534,#6532,#3541,.T.);
#7887=EDGE_CURVE('',#6534,#6535,#3542,.T.);
#7888=EDGE_CURVE('',#6533,#6535,#3543,.T.);
#7889=EDGE_CURVE('',#6536,#6534,#3544,.T.);
#7890=EDGE_CURVE('',#6536,#6537,#3545,.T.);
#7891=EDGE_CURVE('',#6535,#6537,#3546,.T.);
#7892=EDGE_CURVE('',#6538,#6536,#3547,.T.);
#7893=EDGE_CURVE('',#6539,#6538,#3548,.T.);
#7894=EDGE_CURVE('',#6537,#6539,#3549,.T.);
#7895=EDGE_CURVE('',#6540,#6540,#5946,.T.);
#7896=EDGE_CURVE('',#6540,#6541,#3550,.T.);
#7897=EDGE_CURVE('',#6541,#6541,#5947,.T.);
#7898=EDGE_CURVE('',#6478,#6542,#3551,.T.);
#7899=EDGE_CURVE('',#6542,#6543,#3552,.T.);
#7900=EDGE_CURVE('',#6479,#6543,#3553,.T.);
#7901=EDGE_CURVE('',#6544,#6463,#3554,.T.);
#7902=EDGE_CURVE('',#6545,#6544,#3555,.T.);
#7903=EDGE_CURVE('',#6545,#6461,#3556,.T.);
#7904=EDGE_CURVE('',#6498,#6545,#3557,.T.);
#7905=EDGE_CURVE('',#6499,#6544,#3558,.T.);
#7906=EDGE_CURVE('',#6546,#6483,#3559,.T.);
#7907=EDGE_CURVE('',#6547,#6546,#3560,.T.);
#7908=EDGE_CURVE('',#6547,#6481,#3561,.T.);
#7909=EDGE_CURVE('',#6518,#6547,#3562,.T.);
#7910=EDGE_CURVE('',#6519,#6546,#3563,.T.);
#7911=EDGE_CURVE('',#6548,#6503,#3564,.T.);
#7912=EDGE_CURVE('',#6549,#6548,#3565,.T.);
#7913=EDGE_CURVE('',#6549,#6501,#3566,.T.);
#7914=EDGE_CURVE('',#6538,#6549,#3567,.T.);
#7915=EDGE_CURVE('',#6539,#6548,#3568,.T.);
#7916=EDGE_CURVE('',#6543,#6523,#3569,.T.);
#7917=EDGE_CURVE('',#6542,#6521,#3570,.T.);
#7918=EDGE_CURVE('',#6550,#6551,#3571,.T.);
#7919=EDGE_CURVE('',#6552,#6550,#3572,.T.);
#7920=EDGE_CURVE('',#6553,#6552,#3573,.T.);
#7921=EDGE_CURVE('',#6551,#6553,#3574,.T.);
#7922=EDGE_CURVE('',#6552,#6554,#3575,.T.);
#7923=EDGE_CURVE('',#6555,#6554,#3576,.T.);
#7924=EDGE_CURVE('',#6553,#6555,#3577,.T.);
#7925=EDGE_CURVE('',#6554,#6556,#3578,.T.);
#7926=EDGE_CURVE('',#6556,#6557,#3579,.T.);
#7927=EDGE_CURVE('',#6557,#6555,#3580,.T.);
#7928=EDGE_CURVE('',#6558,#6558,#5948,.T.);
#7929=EDGE_CURVE('',#6559,#6550,#3581,.T.);
#7930=EDGE_CURVE('',#6560,#6559,#3582,.T.);
#7931=EDGE_CURVE('',#6560,#6561,#3583,.T.);
#7932=EDGE_CURVE('',#6562,#6561,#3584,.T.);
#7933=EDGE_CURVE('',#6562,#6563,#3585,.T.);
#7934=EDGE_CURVE('',#6563,#6564,#3586,.T.);
#7935=EDGE_CURVE('',#6564,#6556,#3587,.T.);
#7936=EDGE_CURVE('',#6564,#6565,#3588,.T.);
#7937=EDGE_CURVE('',#6565,#6557,#3589,.T.);
#7938=EDGE_CURVE('',#6566,#6563,#3590,.T.);
#7939=EDGE_CURVE('',#6565,#6566,#3591,.T.);
#7940=EDGE_CURVE('',#6567,#6566,#3592,.T.);
#7941=EDGE_CURVE('',#6568,#6567,#3593,.T.);
#7942=EDGE_CURVE('',#6568,#6569,#3594,.T.);
#7943=EDGE_CURVE('',#6570,#6569,#3595,.T.);
#7944=EDGE_CURVE('',#6570,#6551,#3596,.T.);
#7945=EDGE_CURVE('',#6567,#6562,#3597,.T.);
#7946=EDGE_CURVE('',#6561,#6571,#3598,.T.);
#7947=EDGE_CURVE('',#6571,#6572,#638,.T.);
#7948=EDGE_CURVE('',#6572,#6568,#3599,.T.);
#7949=EDGE_CURVE('',#6573,#6571,#5949,.F.);
#7950=EDGE_CURVE('',#6573,#6558,#3600,.T.);
#7951=EDGE_CURVE('',#6574,#6573,#5950,.F.);
#7952=EDGE_CURVE('',#6575,#6574,#639,.T.);
#7953=EDGE_CURVE('',#6572,#6575,#5951,.F.);
#7954=EDGE_CURVE('',#6574,#6560,#3601,.T.);
#7955=EDGE_CURVE('',#6569,#6575,#3602,.T.);
#7956=EDGE_CURVE('',#6559,#6570,#3603,.T.);
#7957=EDGE_CURVE('',#6576,#6576,#5952,.T.);
#7958=EDGE_CURVE('',#6576,#6577,#3604,.T.);
#7959=EDGE_CURVE('',#6577,#6577,#5953,.T.);
#7960=EDGE_CURVE('',#6577,#6578,#3605,.T.);
#7961=EDGE_CURVE('',#6578,#6578,#5954,.T.);
#7962=EDGE_CURVE('',#6579,#6579,#5955,.T.);
#7963=EDGE_CURVE('',#6579,#6580,#3606,.T.);
#7964=EDGE_CURVE('',#6580,#6580,#5956,.T.);
#7965=EDGE_CURVE('',#6581,#6581,#5957,.T.);
#7966=EDGE_CURVE('',#6581,#6582,#3607,.T.);
#7967=EDGE_CURVE('',#6582,#6582,#5958,.T.);
#7968=EDGE_CURVE('',#6583,#6583,#5959,.T.);
#7969=EDGE_CURVE('',#6584,#6584,#5960,.T.);
#7970=EDGE_CURVE('',#6584,#6585,#3608,.T.);
#7971=EDGE_CURVE('',#6585,#6585,#5961,.T.);
#7972=EDGE_CURVE('',#6586,#6586,#5962,.T.);
#7973=EDGE_CURVE('',#6587,#6587,#5963,.T.);
#7974=EDGE_CURVE('',#6587,#6588,#3609,.T.);
#7975=EDGE_CURVE('',#6588,#6588,#5964,.T.);
#7976=EDGE_CURVE('',#6589,#6589,#5965,.T.);
#7977=EDGE_CURVE('',#6590,#6590,#5966,.T.);
#7978=EDGE_CURVE('',#6590,#6591,#3610,.T.);
#7979=EDGE_CURVE('',#6591,#6591,#5967,.T.);
#7980=EDGE_CURVE('',#6592,#6592,#5968,.T.);
#7981=EDGE_CURVE('',#6593,#6593,#5969,.T.);
#7982=EDGE_CURVE('',#6593,#6583,#3611,.T.);
#7983=EDGE_CURVE('',#6594,#6594,#5970,.T.);
#7984=EDGE_CURVE('',#6594,#6586,#3612,.T.);
#7985=EDGE_CURVE('',#6595,#6595,#5971,.T.);
#7986=EDGE_CURVE('',#6595,#6589,#3613,.T.);
#7987=EDGE_CURVE('',#6596,#6596,#5972,.T.);
#7988=EDGE_CURVE('',#6596,#6592,#3614,.T.);
#7989=EDGE_CURVE('',#6597,#6598,#3615,.T.);
#7990=EDGE_CURVE('',#6598,#6599,#3616,.T.);
#7991=EDGE_CURVE('',#6600,#6599,#3617,.T.);
#7992=EDGE_CURVE('',#6597,#6600,#3618,.T.);
#7993=EDGE_CURVE('',#6601,#6597,#3619,.T.);
#7994=EDGE_CURVE('',#6602,#6600,#3620,.T.);
#7995=EDGE_CURVE('',#6601,#6602,#3621,.T.);
#7996=EDGE_CURVE('',#6603,#6601,#3622,.T.);
#7997=EDGE_CURVE('',#6604,#6602,#3623,.T.);
#7998=EDGE_CURVE('',#6603,#6604,#3624,.T.);
#7999=EDGE_CURVE('',#6605,#6603,#3625,.T.);
#8000=EDGE_CURVE('',#6606,#6604,#3626,.T.);
#8001=EDGE_CURVE('',#6605,#6606,#3627,.T.);
#8002=EDGE_CURVE('',#6607,#6605,#3628,.T.);
#8003=EDGE_CURVE('',#6608,#6606,#3629,.T.);
#8004=EDGE_CURVE('',#6607,#6608,#3630,.T.);
#8005=EDGE_CURVE('',#6609,#6607,#3631,.T.);
#8006=EDGE_CURVE('',#6610,#6608,#3632,.T.);
#8007=EDGE_CURVE('',#6609,#6610,#3633,.T.);
#8008=EDGE_CURVE('',#6611,#6609,#3634,.T.);
#8009=EDGE_CURVE('',#6612,#6610,#3635,.T.);
#8010=EDGE_CURVE('',#6611,#6612,#3636,.T.);
#8011=EDGE_CURVE('',#6613,#6611,#3637,.T.);
#8012=EDGE_CURVE('',#6614,#6612,#3638,.T.);
#8013=EDGE_CURVE('',#6613,#6614,#3639,.T.);
#8014=EDGE_CURVE('',#6615,#6613,#3640,.T.);
#8015=EDGE_CURVE('',#6616,#6614,#3641,.T.);
#8016=EDGE_CURVE('',#6615,#6616,#3642,.T.);
#8017=EDGE_CURVE('',#6617,#6615,#3643,.T.);
#8018=EDGE_CURVE('',#6618,#6616,#3644,.T.);
#8019=EDGE_CURVE('',#6617,#6618,#3645,.T.);
#8020=EDGE_CURVE('',#6619,#6617,#3646,.T.);
#8021=EDGE_CURVE('',#6620,#6618,#3647,.T.);
#8022=EDGE_CURVE('',#6619,#6620,#3648,.T.);
#8023=EDGE_CURVE('',#6598,#6619,#3649,.T.);
#8024=EDGE_CURVE('',#6599,#6620,#3650,.T.);
#8025=EDGE_CURVE('',#6621,#6621,#5973,.T.);
#8026=EDGE_CURVE('',#6622,#6622,#5974,.T.);
#8027=EDGE_CURVE('',#6622,#6621,#3651,.T.);
#8028=EDGE_CURVE('',#6623,#6623,#5975,.T.);
#8029=EDGE_CURVE('',#6623,#6622,#3652,.T.);
#8030=EDGE_CURVE('',#6624,#6624,#5976,.T.);
#8031=EDGE_CURVE('',#6624,#6623,#3653,.T.);
#8032=EDGE_CURVE('',#6625,#6625,#5977,.T.);
#8033=EDGE_CURVE('',#6626,#6626,#5978,.F.);
#8034=EDGE_CURVE('',#6626,#6625,#3654,.T.);
#8035=EDGE_CURVE('',#6627,#6627,#5979,.F.);
#8036=EDGE_CURVE('',#6627,#6626,#3655,.T.);
#8037=EDGE_CURVE('',#6628,#6628,#5980,.T.);
#8038=EDGE_CURVE('',#6628,#6627,#3656,.T.);
#8039=EDGE_CURVE('',#6629,#6630,#3657,.T.);
#8040=EDGE_CURVE('',#6630,#6631,#3658,.T.);
#8041=EDGE_CURVE('',#6631,#6632,#3659,.T.);
#8042=EDGE_CURVE('',#6629,#6632,#3660,.T.);
#8043=EDGE_CURVE('',#6630,#6633,#3661,.T.);
#8044=EDGE_CURVE('',#6633,#6634,#3662,.T.);
#8045=EDGE_CURVE('',#6634,#6631,#3663,.T.);
#8046=EDGE_CURVE('',#6633,#6635,#3664,.T.);
#8047=EDGE_CURVE('',#6635,#6636,#3665,.T.);
#8048=EDGE_CURVE('',#6636,#6634,#3666,.T.);
#8049=EDGE_CURVE('',#6635,#6637,#3667,.T.);
#8050=EDGE_CURVE('',#6637,#6638,#3668,.T.);
#8051=EDGE_CURVE('',#6638,#6636,#3669,.T.);
#8052=EDGE_CURVE('',#6637,#6639,#3670,.T.);
#8053=EDGE_CURVE('',#6639,#6640,#3671,.T.);
#8054=EDGE_CURVE('',#6640,#6638,#3672,.T.);
#8055=EDGE_CURVE('',#6639,#6629,#3673,.T.);
#8056=EDGE_CURVE('',#6632,#6640,#3674,.T.);
#8057=EDGE_CURVE('',#6641,#6642,#5981,.T.);
#8058=EDGE_CURVE('',#6642,#6641,#5982,.T.);
#8059=EDGE_CURVE('',#6642,#6643,#5983,.T.);
#8060=EDGE_CURVE('',#6644,#6643,#5984,.T.);
#8061=EDGE_CURVE('',#6643,#6644,#5985,.T.);
#8062=EDGE_CURVE('',#6644,#6645,#3675,.T.);
#8063=EDGE_CURVE('',#6645,#6645,#5986,.T.);
#8064=EDGE_CURVE('',#6646,#6646,#5987,.T.);
#8065=EDGE_CURVE('',#6646,#6647,#3676,.T.);
#8066=EDGE_CURVE('',#6647,#6647,#5988,.T.);
#8067=EDGE_CURVE('',#6647,#6648,#3677,.T.);
#8068=EDGE_CURVE('',#6648,#6648,#5989,.T.);
#8069=EDGE_CURVE('',#6649,#6649,#5990,.T.);
#8070=EDGE_CURVE('',#6649,#6641,#3678,.T.);
#8071=EDGE_CURVE('',#6650,#6650,#5991,.T.);
#8072=EDGE_CURVE('',#6650,#6646,#3679,.T.);
#8073=EDGE_CURVE('',#6651,#6652,#5992,.T.);
#8074=EDGE_CURVE('',#6652,#6651,#5993,.T.);
#8075=EDGE_CURVE('',#6652,#6653,#5994,.T.);
#8076=EDGE_CURVE('',#6654,#6653,#5995,.T.);
#8077=EDGE_CURVE('',#6653,#6654,#5996,.T.);
#8078=EDGE_CURVE('',#6655,#6655,#5997,.T.);
#8079=EDGE_CURVE('',#6655,#6654,#3680,.T.);
#8080=EDGE_CURVE('',#6656,#6656,#5998,.T.);
#8081=EDGE_CURVE('',#6657,#6657,#5999,.T.);
#8082=EDGE_CURVE('',#6658,#6658,#6000,.T.);
#8083=EDGE_CURVE('',#6658,#6656,#3681,.T.);
#8084=EDGE_CURVE('',#6659,#6659,#6001,.T.);
#8085=EDGE_CURVE('',#6659,#6658,#3682,.T.);
#8086=EDGE_CURVE('',#6660,#6660,#6002,.T.);
#8087=EDGE_CURVE('',#6660,#6659,#3683,.T.);
#8088=EDGE_CURVE('',#6651,#6657,#3684,.T.);
#8089=EDGE_CURVE('',#6661,#6662,#6003,.T.);
#8090=EDGE_CURVE('',#6663,#6664,#6004,.T.);
#8091=EDGE_CURVE('',#6665,#6666,#6005,.T.);
#8092=EDGE_CURVE('',#6667,#6668,#6006,.T.);
#8093=EDGE_CURVE('',#6669,#6670,#6007,.T.);
#8094=EDGE_CURVE('',#6671,#6672,#6008,.T.);
#8095=EDGE_CURVE('',#6673,#6674,#6009,.T.);
#8096=EDGE_CURVE('',#6675,#6676,#575,.T.);
#8097=EDGE_CURVE('',#6677,#6675,#6010,.T.);
#8098=EDGE_CURVE('',#6678,#6677,#576,.T.);
#8099=EDGE_CURVE('',#6676,#6678,#6011,.T.);
#8100=EDGE_CURVE('',#6679,#6677,#6012,.T.);
#8101=EDGE_CURVE('',#6679,#6680,#577,.T.);
#8102=EDGE_CURVE('',#6681,#6680,#6013,.T.);
#8103=EDGE_CURVE('',#6681,#6682,#578,.T.);
#8104=EDGE_CURVE('',#6683,#6682,#6014,.T.);
#8105=EDGE_CURVE('',#6683,#6684,#3685,.T.);
#8106=EDGE_CURVE('',#6684,#6684,#6015,.T.);
#8107=EDGE_CURVE('',#6685,#6683,#6016,.T.);
#8108=EDGE_CURVE('',#6685,#6686,#579,.T.);
#8109=EDGE_CURVE('',#6687,#6686,#6017,.T.);
#8110=EDGE_CURVE('',#6687,#6688,#580,.T.);
#8111=EDGE_CURVE('',#6689,#6688,#6018,.T.);
#8112=EDGE_CURVE('',#6689,#6690,#581,.T.);
#8113=EDGE_CURVE('',#6691,#6690,#6019,.T.);
#8114=EDGE_CURVE('',#6691,#6692,#582,.T.);
#8115=EDGE_CURVE('',#6678,#6692,#6020,.T.);
#8116=EDGE_CURVE('',#6675,#6693,#6021,.T.);
#8117=EDGE_CURVE('',#6693,#6679,#6022,.T.);
#8118=EDGE_CURVE('',#6694,#6693,#583,.T.);
#8119=EDGE_CURVE('',#6680,#6694,#6023,.T.);
#8120=EDGE_CURVE('',#6694,#6695,#6024,.T.);
#8121=EDGE_CURVE('',#6695,#6681,#6025,.T.);
#8122=EDGE_CURVE('',#6696,#6695,#584,.T.);
#8123=EDGE_CURVE('',#6682,#6696,#6026,.T.);
#8124=EDGE_CURVE('',#6696,#6697,#6027,.T.);
#8125=EDGE_CURVE('',#6697,#6698,#6028,.T.);
#8126=EDGE_CURVE('',#6698,#6685,#6029,.T.);
#8127=EDGE_CURVE('',#6699,#6698,#585,.T.);
#8128=EDGE_CURVE('',#6686,#6699,#6030,.T.);
#8129=EDGE_CURVE('',#6699,#6700,#6031,.T.);
#8130=EDGE_CURVE('',#6700,#6687,#6032,.T.);
#8131=EDGE_CURVE('',#6701,#6700,#586,.T.);
#8132=EDGE_CURVE('',#6688,#6701,#6033,.T.);
#8133=EDGE_CURVE('',#6701,#6702,#6034,.T.);
#8134=EDGE_CURVE('',#6702,#6689,#6035,.T.);
#8135=EDGE_CURVE('',#6703,#6702,#587,.T.);
#8136=EDGE_CURVE('',#6690,#6703,#6036,.T.);
#8137=EDGE_CURVE('',#6704,#6704,#6037,.T.);
#8138=EDGE_CURVE('',#6704,#6697,#3686,.T.);
#8139=EDGE_CURVE('',#6705,#6676,#6038,.T.);
#8140=EDGE_CURVE('',#6705,#6706,#588,.T.);
#8141=EDGE_CURVE('',#6703,#6706,#6039,.T.);
#8142=EDGE_CURVE('',#6692,#6705,#6040,.T.);
#8143=EDGE_CURVE('',#6706,#6691,#6041,.T.);
#8144=EDGE_CURVE('',#6707,#6707,#6042,.T.);
#8145=EDGE_CURVE('',#6708,#6708,#6043,.T.);
#8146=EDGE_CURVE('',#6709,#6709,#6044,.T.);
#8147=EDGE_CURVE('',#6709,#6707,#3687,.T.);
#8148=EDGE_CURVE('',#6710,#6710,#6045,.T.);
#8149=EDGE_CURVE('',#6710,#6708,#3688,.T.);
#8150=EDGE_CURVE('',#6711,#6711,#6046,.T.);
#8151=EDGE_CURVE('',#6712,#6712,#6047,.T.);
#8152=EDGE_CURVE('',#6713,#6713,#6048,.T.);
#8153=EDGE_CURVE('',#6713,#6711,#3689,.T.);
#8154=EDGE_CURVE('',#6714,#6714,#6049,.T.);
#8155=EDGE_CURVE('',#6714,#6712,#3690,.T.);
#8156=EDGE_CURVE('',#6715,#6716,#3691,.T.);
#8157=EDGE_CURVE('',#6716,#6717,#3692,.T.);
#8158=EDGE_CURVE('',#6717,#6718,#3693,.T.);
#8159=EDGE_CURVE('',#6715,#6718,#3694,.T.);
#8160=EDGE_CURVE('',#6716,#6719,#3695,.T.);
#8161=EDGE_CURVE('',#6719,#6720,#3696,.T.);
#8162=EDGE_CURVE('',#6720,#6717,#3697,.T.);
#8163=EDGE_CURVE('',#6719,#6721,#3698,.T.);
#8164=EDGE_CURVE('',#6721,#6722,#3699,.T.);
#8165=EDGE_CURVE('',#6722,#6720,#3700,.T.);
#8166=EDGE_CURVE('',#6721,#6723,#3701,.T.);
#8167=EDGE_CURVE('',#6723,#6724,#3702,.T.);
#8168=EDGE_CURVE('',#6724,#6722,#3703,.T.);
#8169=EDGE_CURVE('',#6723,#6725,#3704,.T.);
#8170=EDGE_CURVE('',#6725,#6726,#3705,.T.);
#8171=EDGE_CURVE('',#6726,#6724,#3706,.T.);
#8172=EDGE_CURVE('',#6725,#6715,#3707,.T.);
#8173=EDGE_CURVE('',#6718,#6726,#3708,.T.);
#8174=EDGE_CURVE('',#6727,#6727,#6050,.T.);
#8175=EDGE_CURVE('',#6728,#6728,#6051,.T.);
#8176=EDGE_CURVE('',#6729,#6729,#6052,.T.);
#8177=EDGE_CURVE('',#6729,#6728,#3709,.T.);
#8178=EDGE_CURVE('',#6730,#6730,#6053,.T.);
#8179=EDGE_CURVE('',#6730,#6729,#3710,.T.);
#8180=EDGE_CURVE('',#6731,#6731,#6054,.T.);
#8181=EDGE_CURVE('',#6731,#6730,#3711,.T.);
#8182=EDGE_CURVE('',#6732,#6732,#6055,.T.);
#8183=EDGE_CURVE('',#6733,#6733,#6056,.F.);
#8184=EDGE_CURVE('',#6733,#6732,#3712,.T.);
#8185=EDGE_CURVE('',#6727,#6733,#3713,.T.);
#8186=EDGE_CURVE('',#6734,#6734,#6057,.T.);
#8187=EDGE_CURVE('',#6734,#6735,#3714,.T.);
#8188=EDGE_CURVE('',#6735,#6735,#6058,.T.);
#8189=EDGE_CURVE('',#6736,#6736,#6059,.T.);
#8190=EDGE_CURVE('',#6736,#6737,#3715,.T.);
#8191=EDGE_CURVE('',#6737,#6737,#6060,.T.);
#8192=EDGE_CURVE('',#6738,#6738,#6061,.T.);
#8193=EDGE_CURVE('',#6738,#6739,#3716,.T.);
#8194=EDGE_CURVE('',#6739,#6739,#6062,.T.);
#8195=EDGE_CURVE('',#6740,#6740,#6063,.T.);
#8196=EDGE_CURVE('',#6740,#6741,#3717,.T.);
#8197=EDGE_CURVE('',#6741,#6741,#6064,.T.);
#8198=EDGE_CURVE('',#6742,#6742,#6065,.T.);
#8199=EDGE_CURVE('',#6742,#6743,#3718,.T.);
#8200=EDGE_CURVE('',#6743,#6743,#6066,.T.);
#8201=EDGE_CURVE('',#6744,#6744,#6067,.T.);
#8202=EDGE_CURVE('',#6744,#6745,#3719,.T.);
#8203=EDGE_CURVE('',#6745,#6745,#6068,.T.);
#8204=EDGE_CURVE('',#6746,#6746,#6069,.T.);
#8205=EDGE_CURVE('',#6746,#6747,#3720,.T.);
#8206=EDGE_CURVE('',#6747,#6747,#6070,.T.);
#8207=EDGE_CURVE('',#6748,#6748,#6071,.T.);
#8208=EDGE_CURVE('',#6748,#6749,#3721,.T.);
#8209=EDGE_CURVE('',#6749,#6749,#6072,.T.);
#8210=EDGE_CURVE('',#6750,#6751,#3722,.T.);
#8211=EDGE_CURVE('',#6751,#6752,#3723,.T.);
#8212=EDGE_CURVE('',#6753,#6752,#3724,.T.);
#8213=EDGE_CURVE('',#6750,#6753,#3725,.T.);
#8214=EDGE_CURVE('',#6754,#6750,#3726,.T.);
#8215=EDGE_CURVE('',#6755,#6753,#3727,.T.);
#8216=EDGE_CURVE('',#6754,#6755,#3728,.T.);
#8217=EDGE_CURVE('',#6756,#6754,#3729,.T.);
#8218=EDGE_CURVE('',#6757,#6755,#3730,.T.);
#8219=EDGE_CURVE('',#6756,#6757,#3731,.T.);
#8220=EDGE_CURVE('',#6751,#6756,#3732,.T.);
#8221=EDGE_CURVE('',#6752,#6757,#3733,.T.);
#8222=EDGE_CURVE('',#6758,#6758,#6073,.T.);
#8223=EDGE_CURVE('',#6758,#6759,#3734,.T.);
#8224=EDGE_CURVE('',#6759,#6759,#6074,.T.);
#8225=EDGE_CURVE('',#6760,#6760,#6075,.T.);
#8226=EDGE_CURVE('',#6760,#6761,#3735,.T.);
#8227=EDGE_CURVE('',#6761,#6761,#6076,.T.);
#8228=EDGE_CURVE('',#6762,#6762,#6077,.T.);
#8229=EDGE_CURVE('',#6762,#6763,#3736,.T.);
#8230=EDGE_CURVE('',#6763,#6763,#6078,.T.);
#8231=EDGE_CURVE('',#6764,#6764,#6079,.T.);
#8232=EDGE_CURVE('',#6764,#6765,#3737,.T.);
#8233=EDGE_CURVE('',#6765,#6765,#6080,.T.);
#8234=EDGE_CURVE('',#6766,#6767,#3738,.T.);
#8235=EDGE_CURVE('',#6766,#6768,#3739,.T.);
#8236=EDGE_CURVE('',#6769,#6768,#3740,.T.);
#8237=EDGE_CURVE('',#6767,#6769,#3741,.T.);
#8238=EDGE_CURVE('',#6767,#6770,#3742,.T.);
#8239=EDGE_CURVE('',#6771,#6769,#3743,.T.);
#8240=EDGE_CURVE('',#6770,#6771,#3744,.T.);
#8241=EDGE_CURVE('',#6770,#6772,#3745,.T.);
#8242=EDGE_CURVE('',#6773,#6771,#3746,.T.);
#8243=EDGE_CURVE('',#6772,#6773,#3747,.T.);
#8244=EDGE_CURVE('',#6772,#6774,#3748,.T.);
#8245=EDGE_CURVE('',#6775,#6773,#3749,.T.);
#8246=EDGE_CURVE('',#6774,#6775,#3750,.T.);
#8247=EDGE_CURVE('',#6774,#6776,#3751,.T.);
#8248=EDGE_CURVE('',#6777,#6775,#3752,.T.);
#8249=EDGE_CURVE('',#6776,#6777,#3753,.T.);
#8250=EDGE_CURVE('',#6776,#6778,#3754,.T.);
#8251=EDGE_CURVE('',#6779,#6777,#3755,.T.);
#8252=EDGE_CURVE('',#6778,#6779,#3756,.T.);
#8253=EDGE_CURVE('',#6778,#6780,#3757,.T.);
#8254=EDGE_CURVE('',#6781,#6779,#3758,.T.);
#8255=EDGE_CURVE('',#6780,#6781,#3759,.T.);
#8256=EDGE_CURVE('',#6780,#6782,#3760,.T.);
#8257=EDGE_CURVE('',#6783,#6781,#3761,.T.);
#8258=EDGE_CURVE('',#6782,#6783,#3762,.T.);
#8259=EDGE_CURVE('',#6782,#6784,#3763,.T.);
#8260=EDGE_CURVE('',#6785,#6783,#3764,.T.);
#8261=EDGE_CURVE('',#6784,#6785,#3765,.T.);
#8262=EDGE_CURVE('',#6784,#6786,#3766,.T.);
#8263=EDGE_CURVE('',#6787,#6785,#3767,.T.);
#8264=EDGE_CURVE('',#6786,#6787,#3768,.T.);
#8265=EDGE_CURVE('',#6786,#6788,#3769,.T.);
#8266=EDGE_CURVE('',#6789,#6787,#3770,.T.);
#8267=EDGE_CURVE('',#6788,#6789,#3771,.T.);
#8268=EDGE_CURVE('',#6788,#6790,#3772,.T.);
#8269=EDGE_CURVE('',#6791,#6789,#3773,.T.);
#8270=EDGE_CURVE('',#6790,#6791,#3774,.T.);
#8271=EDGE_CURVE('',#6790,#6792,#3775,.T.);
#8272=EDGE_CURVE('',#6793,#6791,#3776,.T.);
#8273=EDGE_CURVE('',#6792,#6793,#3777,.T.);
#8274=EDGE_CURVE('',#6792,#6794,#3778,.T.);
#8275=EDGE_CURVE('',#6795,#6793,#3779,.T.);
#8276=EDGE_CURVE('',#6794,#6795,#3780,.T.);
#8277=EDGE_CURVE('',#6794,#6796,#3781,.T.);
#8278=EDGE_CURVE('',#6797,#6795,#3782,.T.);
#8279=EDGE_CURVE('',#6796,#6797,#3783,.T.);
#8280=EDGE_CURVE('',#6796,#6798,#3784,.T.);
#8281=EDGE_CURVE('',#6799,#6797,#3785,.T.);
#8282=EDGE_CURVE('',#6798,#6799,#3786,.T.);
#8283=EDGE_CURVE('',#6798,#6800,#3787,.T.);
#8284=EDGE_CURVE('',#6801,#6799,#3788,.T.);
#8285=EDGE_CURVE('',#6800,#6801,#3789,.T.);
#8286=EDGE_CURVE('',#6800,#6802,#3790,.T.);
#8287=EDGE_CURVE('',#6803,#6801,#3791,.T.);
#8288=EDGE_CURVE('',#6802,#6803,#3792,.T.);
#8289=EDGE_CURVE('',#6802,#6804,#3793,.T.);
#8290=EDGE_CURVE('',#6805,#6803,#3794,.T.);
#8291=EDGE_CURVE('',#6804,#6805,#3795,.T.);
#8292=EDGE_CURVE('',#6804,#6806,#3796,.T.);
#8293=EDGE_CURVE('',#6807,#6805,#3797,.T.);
#8294=EDGE_CURVE('',#6806,#6807,#3798,.T.);
#8295=EDGE_CURVE('',#6806,#6808,#3799,.T.);
#8296=EDGE_CURVE('',#6809,#6807,#3800,.T.);
#8297=EDGE_CURVE('',#6808,#6809,#3801,.T.);
#8298=EDGE_CURVE('',#6808,#6810,#3802,.T.);
#8299=EDGE_CURVE('',#6811,#6809,#3803,.T.);
#8300=EDGE_CURVE('',#6810,#6811,#3804,.T.);
#8301=EDGE_CURVE('',#6810,#6812,#3805,.T.);
#8302=EDGE_CURVE('',#6813,#6811,#3806,.T.);
#8303=EDGE_CURVE('',#6812,#6813,#3807,.T.);
#8304=EDGE_CURVE('',#6812,#6814,#3808,.T.);
#8305=EDGE_CURVE('',#6815,#6813,#3809,.T.);
#8306=EDGE_CURVE('',#6814,#6815,#3810,.T.);
#8307=EDGE_CURVE('',#6814,#6816,#3811,.T.);
#8308=EDGE_CURVE('',#6817,#6815,#3812,.T.);
#8309=EDGE_CURVE('',#6816,#6817,#3813,.T.);
#8310=EDGE_CURVE('',#6816,#6818,#3814,.T.);
#8311=EDGE_CURVE('',#6819,#6817,#3815,.T.);
#8312=EDGE_CURVE('',#6818,#6819,#3816,.T.);
#8313=EDGE_CURVE('',#6818,#6820,#3817,.T.);
#8314=EDGE_CURVE('',#6821,#6819,#3818,.T.);
#8315=EDGE_CURVE('',#6820,#6821,#3819,.T.);
#8316=EDGE_CURVE('',#6820,#6822,#3820,.T.);
#8317=EDGE_CURVE('',#6823,#6821,#3821,.T.);
#8318=EDGE_CURVE('',#6822,#6823,#3822,.T.);
#8319=EDGE_CURVE('',#6822,#6824,#3823,.T.);
#8320=EDGE_CURVE('',#6825,#6823,#3824,.T.);
#8321=EDGE_CURVE('',#6824,#6825,#3825,.T.);
#8322=EDGE_CURVE('',#6824,#6826,#3826,.T.);
#8323=EDGE_CURVE('',#6827,#6825,#3827,.T.);
#8324=EDGE_CURVE('',#6826,#6827,#3828,.T.);
#8325=EDGE_CURVE('',#6826,#6828,#3829,.T.);
#8326=EDGE_CURVE('',#6829,#6827,#3830,.T.);
#8327=EDGE_CURVE('',#6828,#6829,#3831,.T.);
#8328=EDGE_CURVE('',#6828,#6830,#3832,.T.);
#8329=EDGE_CURVE('',#6831,#6829,#3833,.T.);
#8330=EDGE_CURVE('',#6830,#6831,#3834,.T.);
#8331=EDGE_CURVE('',#6830,#6832,#3835,.T.);
#8332=EDGE_CURVE('',#6833,#6831,#3836,.T.);
#8333=EDGE_CURVE('',#6832,#6833,#3837,.T.);
#8334=EDGE_CURVE('',#6832,#6834,#3838,.T.);
#8335=EDGE_CURVE('',#6835,#6833,#3839,.T.);
#8336=EDGE_CURVE('',#6834,#6835,#3840,.T.);
#8337=EDGE_CURVE('',#6834,#6836,#3841,.T.);
#8338=EDGE_CURVE('',#6837,#6835,#3842,.T.);
#8339=EDGE_CURVE('',#6836,#6837,#3843,.T.);
#8340=EDGE_CURVE('',#6836,#6838,#3844,.T.);
#8341=EDGE_CURVE('',#6839,#6837,#3845,.T.);
#8342=EDGE_CURVE('',#6838,#6839,#3846,.T.);
#8343=EDGE_CURVE('',#6838,#6840,#3847,.T.);
#8344=EDGE_CURVE('',#6841,#6839,#3848,.T.);
#8345=EDGE_CURVE('',#6840,#6841,#3849,.T.);
#8346=EDGE_CURVE('',#6840,#6842,#3850,.T.);
#8347=EDGE_CURVE('',#6843,#6841,#3851,.T.);
#8348=EDGE_CURVE('',#6842,#6843,#3852,.T.);
#8349=EDGE_CURVE('',#6842,#6844,#3853,.T.);
#8350=EDGE_CURVE('',#6845,#6843,#3854,.T.);
#8351=EDGE_CURVE('',#6844,#6845,#3855,.T.);
#8352=EDGE_CURVE('',#6844,#6846,#3856,.T.);
#8353=EDGE_CURVE('',#6847,#6845,#3857,.T.);
#8354=EDGE_CURVE('',#6846,#6847,#3858,.T.);
#8355=EDGE_CURVE('',#6846,#6848,#3859,.T.);
#8356=EDGE_CURVE('',#6849,#6847,#3860,.T.);
#8357=EDGE_CURVE('',#6848,#6849,#3861,.T.);
#8358=EDGE_CURVE('',#6848,#6850,#3862,.T.);
#8359=EDGE_CURVE('',#6851,#6849,#3863,.T.);
#8360=EDGE_CURVE('',#6850,#6851,#3864,.T.);
#8361=EDGE_CURVE('',#6850,#6852,#3865,.T.);
#8362=EDGE_CURVE('',#6853,#6851,#3866,.T.);
#8363=EDGE_CURVE('',#6852,#6853,#3867,.T.);
#8364=EDGE_CURVE('',#6852,#6854,#3868,.T.);
#8365=EDGE_CURVE('',#6855,#6853,#3869,.T.);
#8366=EDGE_CURVE('',#6854,#6855,#3870,.T.);
#8367=EDGE_CURVE('',#6854,#6856,#3871,.T.);
#8368=EDGE_CURVE('',#6857,#6855,#3872,.T.);
#8369=EDGE_CURVE('',#6856,#6857,#3873,.T.);
#8370=EDGE_CURVE('',#6856,#6858,#3874,.T.);
#8371=EDGE_CURVE('',#6859,#6857,#3875,.T.);
#8372=EDGE_CURVE('',#6858,#6859,#3876,.T.);
#8373=EDGE_CURVE('',#6858,#6860,#3877,.T.);
#8374=EDGE_CURVE('',#6861,#6859,#3878,.T.);
#8375=EDGE_CURVE('',#6860,#6861,#3879,.T.);
#8376=EDGE_CURVE('',#6860,#6862,#3880,.T.);
#8377=EDGE_CURVE('',#6863,#6861,#3881,.T.);
#8378=EDGE_CURVE('',#6862,#6863,#3882,.T.);
#8379=EDGE_CURVE('',#6862,#6864,#3883,.T.);
#8380=EDGE_CURVE('',#6865,#6863,#3884,.T.);
#8381=EDGE_CURVE('',#6864,#6865,#3885,.T.);
#8382=EDGE_CURVE('',#6864,#6866,#3886,.T.);
#8383=EDGE_CURVE('',#6867,#6865,#3887,.T.);
#8384=EDGE_CURVE('',#6866,#6867,#3888,.T.);
#8385=EDGE_CURVE('',#6866,#6868,#3889,.T.);
#8386=EDGE_CURVE('',#6869,#6867,#3890,.T.);
#8387=EDGE_CURVE('',#6868,#6869,#3891,.T.);
#8388=EDGE_CURVE('',#6868,#6870,#3892,.T.);
#8389=EDGE_CURVE('',#6871,#6869,#3893,.T.);
#8390=EDGE_CURVE('',#6870,#6871,#3894,.T.);
#8391=EDGE_CURVE('',#6870,#6872,#3895,.T.);
#8392=EDGE_CURVE('',#6873,#6871,#3896,.T.);
#8393=EDGE_CURVE('',#6872,#6873,#3897,.T.);
#8394=EDGE_CURVE('',#6872,#6874,#3898,.T.);
#8395=EDGE_CURVE('',#6875,#6873,#3899,.T.);
#8396=EDGE_CURVE('',#6874,#6875,#3900,.T.);
#8397=EDGE_CURVE('',#6874,#6876,#3901,.T.);
#8398=EDGE_CURVE('',#6877,#6875,#3902,.T.);
#8399=EDGE_CURVE('',#6876,#6877,#3903,.T.);
#8400=EDGE_CURVE('',#6876,#6878,#3904,.T.);
#8401=EDGE_CURVE('',#6879,#6877,#3905,.T.);
#8402=EDGE_CURVE('',#6878,#6879,#3906,.T.);
#8403=EDGE_CURVE('',#6878,#6880,#3907,.T.);
#8404=EDGE_CURVE('',#6881,#6879,#3908,.T.);
#8405=EDGE_CURVE('',#6880,#6881,#3909,.T.);
#8406=EDGE_CURVE('',#6880,#6882,#3910,.T.);
#8407=EDGE_CURVE('',#6883,#6881,#3911,.T.);
#8408=EDGE_CURVE('',#6882,#6883,#3912,.T.);
#8409=EDGE_CURVE('',#6882,#6884,#3913,.T.);
#8410=EDGE_CURVE('',#6885,#6883,#3914,.T.);
#8411=EDGE_CURVE('',#6884,#6885,#3915,.T.);
#8412=EDGE_CURVE('',#6884,#6886,#3916,.T.);
#8413=EDGE_CURVE('',#6887,#6885,#3917,.T.);
#8414=EDGE_CURVE('',#6886,#6887,#3918,.T.);
#8415=EDGE_CURVE('',#6886,#6888,#3919,.T.);
#8416=EDGE_CURVE('',#6889,#6887,#3920,.T.);
#8417=EDGE_CURVE('',#6888,#6889,#3921,.T.);
#8418=EDGE_CURVE('',#6888,#6890,#3922,.T.);
#8419=EDGE_CURVE('',#6891,#6889,#3923,.T.);
#8420=EDGE_CURVE('',#6890,#6891,#3924,.T.);
#8421=EDGE_CURVE('',#6890,#6892,#3925,.T.);
#8422=EDGE_CURVE('',#6893,#6891,#3926,.T.);
#8423=EDGE_CURVE('',#6892,#6893,#3927,.T.);
#8424=EDGE_CURVE('',#6892,#6894,#3928,.T.);
#8425=EDGE_CURVE('',#6895,#6893,#3929,.T.);
#8426=EDGE_CURVE('',#6894,#6895,#3930,.T.);
#8427=EDGE_CURVE('',#6894,#6896,#3931,.T.);
#8428=EDGE_CURVE('',#6897,#6895,#3932,.T.);
#8429=EDGE_CURVE('',#6896,#6897,#3933,.T.);
#8430=EDGE_CURVE('',#6896,#6898,#3934,.T.);
#8431=EDGE_CURVE('',#6899,#6897,#3935,.T.);
#8432=EDGE_CURVE('',#6898,#6899,#3936,.T.);
#8433=EDGE_CURVE('',#6898,#6900,#3937,.T.);
#8434=EDGE_CURVE('',#6901,#6899,#3938,.T.);
#8435=EDGE_CURVE('',#6900,#6901,#3939,.T.);
#8436=EDGE_CURVE('',#6900,#6902,#3940,.T.);
#8437=EDGE_CURVE('',#6903,#6901,#3941,.T.);
#8438=EDGE_CURVE('',#6902,#6903,#3942,.T.);
#8439=EDGE_CURVE('',#6902,#6904,#3943,.T.);
#8440=EDGE_CURVE('',#6905,#6903,#3944,.T.);
#8441=EDGE_CURVE('',#6904,#6905,#3945,.T.);
#8442=EDGE_CURVE('',#6904,#6906,#3946,.T.);
#8443=EDGE_CURVE('',#6907,#6905,#3947,.T.);
#8444=EDGE_CURVE('',#6906,#6907,#3948,.T.);
#8445=EDGE_CURVE('',#6906,#6908,#3949,.T.);
#8446=EDGE_CURVE('',#6909,#6907,#3950,.T.);
#8447=EDGE_CURVE('',#6908,#6909,#3951,.T.);
#8448=EDGE_CURVE('',#6908,#6910,#3952,.T.);
#8449=EDGE_CURVE('',#6911,#6909,#3953,.T.);
#8450=EDGE_CURVE('',#6910,#6911,#3954,.T.);
#8451=EDGE_CURVE('',#6910,#6912,#3955,.T.);
#8452=EDGE_CURVE('',#6913,#6911,#3956,.T.);
#8453=EDGE_CURVE('',#6912,#6913,#3957,.T.);
#8454=EDGE_CURVE('',#6912,#6914,#3958,.T.);
#8455=EDGE_CURVE('',#6915,#6913,#3959,.T.);
#8456=EDGE_CURVE('',#6914,#6915,#3960,.T.);
#8457=EDGE_CURVE('',#6914,#6916,#3961,.T.);
#8458=EDGE_CURVE('',#6917,#6915,#3962,.T.);
#8459=EDGE_CURVE('',#6916,#6917,#3963,.T.);
#8460=EDGE_CURVE('',#6916,#6918,#3964,.T.);
#8461=EDGE_CURVE('',#6919,#6917,#3965,.T.);
#8462=EDGE_CURVE('',#6918,#6919,#3966,.T.);
#8463=EDGE_CURVE('',#6918,#6920,#3967,.T.);
#8464=EDGE_CURVE('',#6921,#6919,#3968,.T.);
#8465=EDGE_CURVE('',#6920,#6921,#3969,.T.);
#8466=EDGE_CURVE('',#6920,#6922,#3970,.T.);
#8467=EDGE_CURVE('',#6923,#6921,#3971,.T.);
#8468=EDGE_CURVE('',#6922,#6923,#3972,.T.);
#8469=EDGE_CURVE('',#6922,#6924,#3973,.T.);
#8470=EDGE_CURVE('',#6925,#6923,#3974,.T.);
#8471=EDGE_CURVE('',#6924,#6925,#3975,.T.);
#8472=EDGE_CURVE('',#6924,#6926,#3976,.T.);
#8473=EDGE_CURVE('',#6927,#6925,#3977,.T.);
#8474=EDGE_CURVE('',#6926,#6927,#3978,.T.);
#8475=EDGE_CURVE('',#6926,#6928,#3979,.T.);
#8476=EDGE_CURVE('',#6929,#6927,#3980,.T.);
#8477=EDGE_CURVE('',#6928,#6929,#3981,.T.);
#8478=EDGE_CURVE('',#6928,#6930,#3982,.T.);
#8479=EDGE_CURVE('',#6931,#6929,#3983,.T.);
#8480=EDGE_CURVE('',#6930,#6931,#3984,.T.);
#8481=EDGE_CURVE('',#6930,#6932,#3985,.T.);
#8482=EDGE_CURVE('',#6933,#6931,#3986,.T.);
#8483=EDGE_CURVE('',#6932,#6933,#3987,.T.);
#8484=EDGE_CURVE('',#6932,#6934,#3988,.T.);
#8485=EDGE_CURVE('',#6935,#6933,#3989,.T.);
#8486=EDGE_CURVE('',#6934,#6935,#3990,.T.);
#8487=EDGE_CURVE('',#6934,#6936,#3991,.T.);
#8488=EDGE_CURVE('',#6937,#6935,#3992,.T.);
#8489=EDGE_CURVE('',#6936,#6937,#3993,.T.);
#8490=EDGE_CURVE('',#6936,#6938,#3994,.T.);
#8491=EDGE_CURVE('',#6939,#6937,#3995,.T.);
#8492=EDGE_CURVE('',#6938,#6939,#3996,.T.);
#8493=EDGE_CURVE('',#6938,#6940,#3997,.T.);
#8494=EDGE_CURVE('',#6941,#6939,#3998,.T.);
#8495=EDGE_CURVE('',#6940,#6941,#3999,.T.);
#8496=EDGE_CURVE('',#6940,#6942,#4000,.T.);
#8497=EDGE_CURVE('',#6943,#6941,#4001,.T.);
#8498=EDGE_CURVE('',#6942,#6943,#4002,.T.);
#8499=EDGE_CURVE('',#6942,#6944,#4003,.T.);
#8500=EDGE_CURVE('',#6945,#6943,#4004,.T.);
#8501=EDGE_CURVE('',#6944,#6945,#4005,.T.);
#8502=EDGE_CURVE('',#6944,#6946,#4006,.T.);
#8503=EDGE_CURVE('',#6947,#6945,#4007,.T.);
#8504=EDGE_CURVE('',#6946,#6947,#4008,.T.);
#8505=EDGE_CURVE('',#6946,#6948,#4009,.T.);
#8506=EDGE_CURVE('',#6949,#6947,#4010,.T.);
#8507=EDGE_CURVE('',#6948,#6949,#4011,.T.);
#8508=EDGE_CURVE('',#6948,#6950,#4012,.T.);
#8509=EDGE_CURVE('',#6951,#6949,#4013,.T.);
#8510=EDGE_CURVE('',#6950,#6951,#4014,.T.);
#8511=EDGE_CURVE('',#6950,#6952,#4015,.T.);
#8512=EDGE_CURVE('',#6953,#6951,#4016,.T.);
#8513=EDGE_CURVE('',#6952,#6953,#4017,.T.);
#8514=EDGE_CURVE('',#6952,#6954,#4018,.T.);
#8515=EDGE_CURVE('',#6955,#6953,#4019,.T.);
#8516=EDGE_CURVE('',#6954,#6955,#4020,.T.);
#8517=EDGE_CURVE('',#6954,#6956,#4021,.T.);
#8518=EDGE_CURVE('',#6957,#6955,#4022,.T.);
#8519=EDGE_CURVE('',#6956,#6957,#4023,.T.);
#8520=EDGE_CURVE('',#6956,#6958,#4024,.T.);
#8521=EDGE_CURVE('',#6959,#6957,#4025,.T.);
#8522=EDGE_CURVE('',#6958,#6959,#4026,.T.);
#8523=EDGE_CURVE('',#6958,#6960,#4027,.T.);
#8524=EDGE_CURVE('',#6961,#6959,#4028,.T.);
#8525=EDGE_CURVE('',#6960,#6961,#4029,.T.);
#8526=EDGE_CURVE('',#6960,#6962,#4030,.T.);
#8527=EDGE_CURVE('',#6963,#6961,#4031,.T.);
#8528=EDGE_CURVE('',#6962,#6963,#4032,.T.);
#8529=EDGE_CURVE('',#6962,#6964,#4033,.T.);
#8530=EDGE_CURVE('',#6965,#6963,#4034,.T.);
#8531=EDGE_CURVE('',#6964,#6965,#4035,.T.);
#8532=EDGE_CURVE('',#6964,#6966,#4036,.T.);
#8533=EDGE_CURVE('',#6967,#6965,#4037,.T.);
#8534=EDGE_CURVE('',#6966,#6967,#4038,.T.);
#8535=EDGE_CURVE('',#6966,#6968,#4039,.T.);
#8536=EDGE_CURVE('',#6969,#6967,#4040,.T.);
#8537=EDGE_CURVE('',#6968,#6969,#4041,.T.);
#8538=EDGE_CURVE('',#6968,#6970,#4042,.T.);
#8539=EDGE_CURVE('',#6971,#6969,#4043,.T.);
#8540=EDGE_CURVE('',#6970,#6971,#4044,.T.);
#8541=EDGE_CURVE('',#6970,#6972,#4045,.T.);
#8542=EDGE_CURVE('',#6973,#6971,#4046,.T.);
#8543=EDGE_CURVE('',#6972,#6973,#4047,.T.);
#8544=EDGE_CURVE('',#6972,#6974,#4048,.T.);
#8545=EDGE_CURVE('',#6975,#6973,#4049,.T.);
#8546=EDGE_CURVE('',#6974,#6975,#4050,.T.);
#8547=EDGE_CURVE('',#6974,#6976,#4051,.T.);
#8548=EDGE_CURVE('',#6977,#6975,#4052,.T.);
#8549=EDGE_CURVE('',#6976,#6977,#4053,.T.);
#8550=EDGE_CURVE('',#6976,#6978,#4054,.T.);
#8551=EDGE_CURVE('',#6979,#6977,#4055,.T.);
#8552=EDGE_CURVE('',#6978,#6979,#4056,.T.);
#8553=EDGE_CURVE('',#6978,#6980,#4057,.T.);
#8554=EDGE_CURVE('',#6981,#6979,#4058,.T.);
#8555=EDGE_CURVE('',#6980,#6981,#4059,.T.);
#8556=EDGE_CURVE('',#6980,#6982,#4060,.T.);
#8557=EDGE_CURVE('',#6983,#6981,#4061,.T.);
#8558=EDGE_CURVE('',#6982,#6983,#4062,.T.);
#8559=EDGE_CURVE('',#6982,#6984,#4063,.T.);
#8560=EDGE_CURVE('',#6985,#6983,#4064,.T.);
#8561=EDGE_CURVE('',#6984,#6985,#4065,.T.);
#8562=EDGE_CURVE('',#6984,#6986,#4066,.T.);
#8563=EDGE_CURVE('',#6987,#6985,#4067,.T.);
#8564=EDGE_CURVE('',#6986,#6987,#4068,.T.);
#8565=EDGE_CURVE('',#6986,#6988,#4069,.T.);
#8566=EDGE_CURVE('',#6989,#6987,#4070,.T.);
#8567=EDGE_CURVE('',#6988,#6989,#4071,.T.);
#8568=EDGE_CURVE('',#6988,#6990,#4072,.T.);
#8569=EDGE_CURVE('',#6991,#6989,#4073,.T.);
#8570=EDGE_CURVE('',#6990,#6991,#4074,.T.);
#8571=EDGE_CURVE('',#6990,#6992,#4075,.T.);
#8572=EDGE_CURVE('',#6993,#6991,#4076,.T.);
#8573=EDGE_CURVE('',#6992,#6993,#4077,.T.);
#8574=EDGE_CURVE('',#6992,#6994,#4078,.T.);
#8575=EDGE_CURVE('',#6995,#6993,#4079,.T.);
#8576=EDGE_CURVE('',#6994,#6995,#4080,.T.);
#8577=EDGE_CURVE('',#6994,#6996,#4081,.T.);
#8578=EDGE_CURVE('',#6997,#6995,#4082,.T.);
#8579=EDGE_CURVE('',#6996,#6997,#4083,.T.);
#8580=EDGE_CURVE('',#6996,#6998,#4084,.T.);
#8581=EDGE_CURVE('',#6999,#6997,#4085,.T.);
#8582=EDGE_CURVE('',#6998,#6999,#4086,.T.);
#8583=EDGE_CURVE('',#6998,#7000,#4087,.T.);
#8584=EDGE_CURVE('',#7001,#6999,#4088,.T.);
#8585=EDGE_CURVE('',#7000,#7001,#4089,.T.);
#8586=EDGE_CURVE('',#7000,#7002,#4090,.T.);
#8587=EDGE_CURVE('',#7003,#7001,#4091,.T.);
#8588=EDGE_CURVE('',#7002,#7003,#4092,.T.);
#8589=EDGE_CURVE('',#7002,#7004,#4093,.T.);
#8590=EDGE_CURVE('',#7005,#7003,#4094,.T.);
#8591=EDGE_CURVE('',#7004,#7005,#4095,.T.);
#8592=EDGE_CURVE('',#7004,#7006,#4096,.T.);
#8593=EDGE_CURVE('',#7007,#7005,#4097,.T.);
#8594=EDGE_CURVE('',#7006,#7007,#4098,.T.);
#8595=EDGE_CURVE('',#7006,#7008,#4099,.T.);
#8596=EDGE_CURVE('',#7009,#7007,#4100,.T.);
#8597=EDGE_CURVE('',#7008,#7009,#4101,.T.);
#8598=EDGE_CURVE('',#7008,#7010,#4102,.T.);
#8599=EDGE_CURVE('',#7011,#7009,#4103,.T.);
#8600=EDGE_CURVE('',#7010,#7011,#4104,.T.);
#8601=EDGE_CURVE('',#7010,#7012,#4105,.T.);
#8602=EDGE_CURVE('',#7013,#7011,#4106,.T.);
#8603=EDGE_CURVE('',#7012,#7013,#4107,.T.);
#8604=EDGE_CURVE('',#7012,#7014,#4108,.T.);
#8605=EDGE_CURVE('',#7015,#7013,#4109,.T.);
#8606=EDGE_CURVE('',#7014,#7015,#4110,.T.);
#8607=EDGE_CURVE('',#7014,#7016,#4111,.T.);
#8608=EDGE_CURVE('',#7017,#7015,#4112,.T.);
#8609=EDGE_CURVE('',#7016,#7017,#4113,.T.);
#8610=EDGE_CURVE('',#7016,#7018,#4114,.T.);
#8611=EDGE_CURVE('',#7019,#7017,#4115,.T.);
#8612=EDGE_CURVE('',#7018,#7019,#4116,.T.);
#8613=EDGE_CURVE('',#7018,#7020,#4117,.T.);
#8614=EDGE_CURVE('',#7021,#7019,#4118,.T.);
#8615=EDGE_CURVE('',#7020,#7021,#4119,.T.);
#8616=EDGE_CURVE('',#7020,#6766,#4120,.T.);
#8617=EDGE_CURVE('',#6768,#7021,#4121,.T.);
#8618=EDGE_CURVE('',#7022,#7023,#4122,.T.);
#8619=EDGE_CURVE('',#7022,#7023,#6081,.T.);
#8620=EDGE_CURVE('',#7024,#7022,#4123,.T.);
#8621=EDGE_CURVE('',#7025,#7024,#6082,.T.);
#8622=EDGE_CURVE('',#7025,#7026,#4124,.T.);
#8623=EDGE_CURVE('',#7026,#7026,#6083,.T.);
#8624=EDGE_CURVE('',#7027,#7025,#6084,.T.);
#8625=EDGE_CURVE('',#7023,#7027,#4125,.T.);
#8626=EDGE_CURVE('',#7028,#7029,#4126,.T.);
#8627=EDGE_CURVE('',#7028,#7029,#6085,.T.);
#8628=EDGE_CURVE('',#7030,#7028,#4127,.T.);
#8629=EDGE_CURVE('',#7031,#7030,#6086,.T.);
#8630=EDGE_CURVE('',#7031,#7032,#4128,.T.);
#8631=EDGE_CURVE('',#7032,#7032,#6087,.T.);
#8632=EDGE_CURVE('',#7033,#7031,#6088,.T.);
#8633=EDGE_CURVE('',#7029,#7033,#4129,.T.);
#8634=EDGE_CURVE('',#7034,#7035,#4130,.T.);
#8635=EDGE_CURVE('',#7034,#7035,#6089,.T.);
#8636=EDGE_CURVE('',#7036,#7034,#4131,.T.);
#8637=EDGE_CURVE('',#7037,#7036,#6090,.T.);
#8638=EDGE_CURVE('',#7037,#7038,#4132,.T.);
#8639=EDGE_CURVE('',#7038,#7038,#6091,.T.);
#8640=EDGE_CURVE('',#7039,#7037,#6092,.T.);
#8641=EDGE_CURVE('',#7035,#7039,#4133,.T.);
#8642=EDGE_CURVE('',#7040,#7041,#4134,.T.);
#8643=EDGE_CURVE('',#7040,#7041,#6093,.T.);
#8644=EDGE_CURVE('',#7042,#7040,#4135,.T.);
#8645=EDGE_CURVE('',#7043,#7042,#6094,.T.);
#8646=EDGE_CURVE('',#7043,#7044,#4136,.T.);
#8647=EDGE_CURVE('',#7044,#7044,#6095,.T.);
#8648=EDGE_CURVE('',#7045,#7043,#6096,.T.);
#8649=EDGE_CURVE('',#7041,#7045,#4137,.T.);
#8650=EDGE_CURVE('',#7027,#7036,#4138,.T.);
#8651=EDGE_CURVE('',#7039,#7046,#4139,.T.);
#8652=EDGE_CURVE('',#7047,#7046,#4140,.T.);
#8653=EDGE_CURVE('',#7047,#7048,#4141,.T.);
#8654=EDGE_CURVE('',#7049,#7048,#4142,.T.);
#8655=EDGE_CURVE('',#7049,#7024,#4143,.T.);
#8656=EDGE_CURVE('',#7033,#7042,#4144,.T.);
#8657=EDGE_CURVE('',#7045,#7050,#4145,.T.);
#8658=EDGE_CURVE('',#7051,#7050,#4146,.T.);
#8659=EDGE_CURVE('',#7052,#7051,#4147,.T.);
#8660=EDGE_CURVE('',#7053,#7052,#4148,.T.);
#8661=EDGE_CURVE('',#7053,#7030,#4149,.T.);
#8662=EDGE_CURVE('',#7046,#7054,#4150,.T.);
#8663=EDGE_CURVE('',#7054,#7055,#4151,.T.);
#8664=EDGE_CURVE('',#7055,#7056,#4152,.T.);
#8665=EDGE_CURVE('',#7056,#7057,#4153,.T.);
#8666=EDGE_CURVE('',#7057,#7053,#4154,.T.);
#8667=EDGE_CURVE('',#7052,#7058,#4155,.T.);
#8668=EDGE_CURVE('',#7058,#7059,#4156,.T.);
#8669=EDGE_CURVE('',#7059,#7060,#4157,.T.);
#8670=EDGE_CURVE('',#7060,#7061,#4158,.T.);
#8671=EDGE_CURVE('',#7061,#7047,#4159,.T.);
#8672=EDGE_CURVE('',#7062,#7049,#4160,.T.);
#8673=EDGE_CURVE('',#7054,#7062,#4161,.T.);
#8674=EDGE_CURVE('',#7063,#7062,#4162,.T.);
#8675=EDGE_CURVE('',#7055,#7063,#4163,.T.);
#8676=EDGE_CURVE('',#7064,#7063,#4164,.T.);
#8677=EDGE_CURVE('',#7056,#7064,#4165,.T.);
#8678=EDGE_CURVE('',#7065,#7064,#4166,.T.);
#8679=EDGE_CURVE('',#7057,#7065,#4167,.T.);
#8680=EDGE_CURVE('',#7050,#7065,#4168,.T.);
#8681=EDGE_CURVE('',#7066,#7051,#4169,.T.);
#8682=EDGE_CURVE('',#7058,#7066,#4170,.T.);
#8683=EDGE_CURVE('',#7067,#7066,#4171,.T.);
#8684=EDGE_CURVE('',#7059,#7067,#4172,.T.);
#8685=EDGE_CURVE('',#7068,#7067,#4173,.T.);
#8686=EDGE_CURVE('',#7060,#7068,#4174,.T.);
#8687=EDGE_CURVE('',#7069,#7068,#4175,.T.);
#8688=EDGE_CURVE('',#7061,#7069,#4176,.T.);
#8689=EDGE_CURVE('',#7048,#7069,#4177,.T.);
#8690=EDGE_CURVE('',#7070,#7071,#4178,.T.);
#8691=EDGE_CURVE('',#7071,#7072,#4179,.T.);
#8692=EDGE_CURVE('',#7073,#7072,#4180,.T.);
#8693=EDGE_CURVE('',#7070,#7073,#4181,.T.);
#8694=EDGE_CURVE('',#7074,#7070,#4182,.T.);
#8695=EDGE_CURVE('',#7075,#7073,#4183,.T.);
#8696=EDGE_CURVE('',#7074,#7075,#4184,.T.);
#8697=EDGE_CURVE('',#7076,#7074,#4185,.T.);
#8698=EDGE_CURVE('',#7077,#7075,#4186,.T.);
#8699=EDGE_CURVE('',#7076,#7077,#4187,.T.);
#8700=EDGE_CURVE('',#7078,#7076,#4188,.T.);
#8701=EDGE_CURVE('',#7079,#7077,#4189,.T.);
#8702=EDGE_CURVE('',#7078,#7079,#4190,.T.);
#8703=EDGE_CURVE('',#7080,#7078,#4191,.T.);
#8704=EDGE_CURVE('',#7081,#7079,#4192,.T.);
#8705=EDGE_CURVE('',#7080,#7081,#4193,.T.);
#8706=EDGE_CURVE('',#7082,#7080,#4194,.T.);
#8707=EDGE_CURVE('',#7083,#7081,#4195,.T.);
#8708=EDGE_CURVE('',#7082,#7083,#4196,.T.);
#8709=EDGE_CURVE('',#7084,#7082,#4197,.T.);
#8710=EDGE_CURVE('',#7085,#7083,#4198,.T.);
#8711=EDGE_CURVE('',#7084,#7085,#4199,.T.);
#8712=EDGE_CURVE('',#7071,#7084,#4200,.T.);
#8713=EDGE_CURVE('',#7072,#7085,#4201,.T.);
#8714=EDGE_CURVE('',#7086,#7087,#4202,.T.);
#8715=EDGE_CURVE('',#7086,#7088,#4203,.T.);
#8716=EDGE_CURVE('',#7089,#7088,#4204,.T.);
#8717=EDGE_CURVE('',#7087,#7089,#4205,.T.);
#8718=EDGE_CURVE('',#7087,#7090,#4206,.T.);
#8719=EDGE_CURVE('',#7091,#7089,#4207,.T.);
#8720=EDGE_CURVE('',#7090,#7091,#4208,.T.);
#8721=EDGE_CURVE('',#7090,#7092,#4209,.T.);
#8722=EDGE_CURVE('',#7093,#7091,#4210,.T.);
#8723=EDGE_CURVE('',#7092,#7093,#4211,.T.);
#8724=EDGE_CURVE('',#7092,#7094,#4212,.T.);
#8725=EDGE_CURVE('',#7095,#7093,#4213,.T.);
#8726=EDGE_CURVE('',#7094,#7095,#4214,.T.);
#8727=EDGE_CURVE('',#7094,#7096,#4215,.T.);
#8728=EDGE_CURVE('',#7097,#7095,#4216,.T.);
#8729=EDGE_CURVE('',#7096,#7097,#4217,.T.);
#8730=EDGE_CURVE('',#7096,#7098,#4218,.T.);
#8731=EDGE_CURVE('',#7099,#7097,#4219,.T.);
#8732=EDGE_CURVE('',#7098,#7099,#4220,.T.);
#8733=EDGE_CURVE('',#7098,#7100,#4221,.T.);
#8734=EDGE_CURVE('',#7101,#7099,#4222,.T.);
#8735=EDGE_CURVE('',#7100,#7101,#4223,.T.);
#8736=EDGE_CURVE('',#7100,#7086,#4224,.T.);
#8737=EDGE_CURVE('',#7088,#7101,#4225,.T.);
#8738=EDGE_CURVE('',#7102,#7103,#4226,.T.);
#8739=EDGE_CURVE('',#7103,#7104,#4227,.T.);
#8740=EDGE_CURVE('',#7104,#7105,#4228,.T.);
#8741=EDGE_CURVE('',#7102,#7105,#4229,.T.);
#8742=EDGE_CURVE('',#7103,#7106,#4230,.T.);
#8743=EDGE_CURVE('',#7106,#7107,#4231,.T.);
#8744=EDGE_CURVE('',#7107,#7104,#4232,.T.);
#8745=EDGE_CURVE('',#7106,#7108,#4233,.T.);
#8746=EDGE_CURVE('',#7108,#7109,#4234,.T.);
#8747=EDGE_CURVE('',#7109,#7107,#4235,.T.);
#8748=EDGE_CURVE('',#7108,#7110,#4236,.T.);
#8749=EDGE_CURVE('',#7110,#7111,#4237,.T.);
#8750=EDGE_CURVE('',#7111,#7109,#4238,.T.);
#8751=EDGE_CURVE('',#7110,#7112,#4239,.T.);
#8752=EDGE_CURVE('',#7112,#7113,#4240,.T.);
#8753=EDGE_CURVE('',#7113,#7111,#4241,.T.);
#8754=EDGE_CURVE('',#7112,#7102,#4242,.T.);
#8755=EDGE_CURVE('',#7105,#7113,#4243,.T.);
#8756=EDGE_CURVE('',#7114,#7114,#6097,.T.);
#8757=EDGE_CURVE('',#7115,#7115,#6098,.T.);
#8758=EDGE_CURVE('',#7116,#7116,#6099,.T.);
#8759=EDGE_CURVE('',#7116,#7115,#4244,.T.);
#8760=EDGE_CURVE('',#7117,#7117,#6100,.T.);
#8761=EDGE_CURVE('',#7117,#7116,#4245,.T.);
#8762=EDGE_CURVE('',#7118,#7118,#6101,.T.);
#8763=EDGE_CURVE('',#7118,#7117,#4246,.T.);
#8764=EDGE_CURVE('',#7119,#7119,#6102,.T.);
#8765=EDGE_CURVE('',#7120,#7120,#6103,.F.);
#8766=EDGE_CURVE('',#7120,#7119,#4247,.T.);
#8767=EDGE_CURVE('',#7114,#7120,#4248,.T.);
#8768=EDGE_CURVE('',#7121,#7122,#4249,.T.);
#8769=EDGE_CURVE('',#7121,#7123,#4250,.T.);
#8770=EDGE_CURVE('',#7124,#7123,#4251,.T.);
#8771=EDGE_CURVE('',#7124,#7122,#4252,.T.);
#8772=EDGE_CURVE('',#7122,#7125,#6104,.T.);
#8773=EDGE_CURVE('',#7126,#7124,#4253,.T.);
#8774=EDGE_CURVE('',#7125,#7126,#4254,.T.);
#8775=EDGE_CURVE('',#7125,#7127,#4255,.T.);
#8776=EDGE_CURVE('',#7126,#7128,#4256,.T.);
#8777=EDGE_CURVE('',#7128,#7127,#4257,.T.);
#8778=EDGE_CURVE('',#7123,#7128,#4258,.T.);
#8779=EDGE_CURVE('',#7127,#7121,#6105,.T.);
#8780=EDGE_CURVE('',#7129,#7129,#6106,.T.);
#8781=EDGE_CURVE('',#7129,#7130,#4259,.T.);
#8782=EDGE_CURVE('',#7130,#7130,#6107,.T.);
#8783=EDGE_CURVE('',#7131,#7131,#6108,.T.);
#8784=EDGE_CURVE('',#7131,#7132,#4260,.T.);
#8785=EDGE_CURVE('',#7132,#7132,#6109,.T.);
#8786=EDGE_CURVE('',#7133,#7134,#4261,.T.);
#8787=EDGE_CURVE('',#7133,#7135,#4262,.T.);
#8788=EDGE_CURVE('',#7136,#7135,#4263,.T.);
#8789=EDGE_CURVE('',#7136,#7134,#4264,.T.);
#8790=EDGE_CURVE('',#7134,#7137,#6110,.T.);
#8791=EDGE_CURVE('',#7138,#7136,#4265,.T.);
#8792=EDGE_CURVE('',#7137,#7138,#4266,.T.);
#8793=EDGE_CURVE('',#7137,#7139,#4267,.T.);
#8794=EDGE_CURVE('',#7138,#7140,#4268,.T.);
#8795=EDGE_CURVE('',#7140,#7139,#4269,.T.);
#8796=EDGE_CURVE('',#7135,#7140,#4270,.T.);
#8797=EDGE_CURVE('',#7139,#7133,#6111,.T.);
#8798=EDGE_CURVE('',#7141,#7141,#6112,.T.);
#8799=EDGE_CURVE('',#7142,#7142,#6113,.T.);
#8800=EDGE_CURVE('',#7143,#7143,#6114,.T.);
#8801=EDGE_CURVE('',#7144,#7144,#6115,.T.);
#8802=EDGE_CURVE('',#7141,#7143,#4271,.T.);
#8803=EDGE_CURVE('',#7144,#7145,#4272,.T.);
#8804=EDGE_CURVE('',#7145,#7145,#6116,.T.);
#8805=EDGE_CURVE('',#7146,#7146,#6117,.T.);
#8806=EDGE_CURVE('',#7146,#7142,#4273,.T.);
#8807=EDGE_CURVE('',#7147,#7147,#6118,.T.);
#8808=EDGE_CURVE('',#7147,#7148,#4274,.T.);
#8809=EDGE_CURVE('',#7148,#7148,#6119,.T.);
#8810=EDGE_CURVE('',#7149,#7149,#6120,.T.);
#8811=EDGE_CURVE('',#7149,#7150,#4275,.T.);
#8812=EDGE_CURVE('',#7150,#7150,#6121,.T.);
#8813=EDGE_CURVE('',#7151,#7151,#6122,.T.);
#8814=EDGE_CURVE('',#7151,#7152,#4276,.T.);
#8815=EDGE_CURVE('',#7152,#7152,#6123,.T.);
#8816=EDGE_CURVE('',#7153,#7153,#6124,.T.);
#8817=EDGE_CURVE('',#7153,#7154,#4277,.T.);
#8818=EDGE_CURVE('',#7154,#7154,#6125,.T.);
#8819=EDGE_CURVE('',#7155,#7155,#6126,.T.);
#8820=EDGE_CURVE('',#7155,#7156,#4278,.T.);
#8821=EDGE_CURVE('',#7156,#7156,#6127,.T.);
#8822=EDGE_CURVE('',#7157,#7157,#6128,.T.);
#8823=EDGE_CURVE('',#7157,#7158,#4279,.T.);
#8824=EDGE_CURVE('',#7158,#7158,#6129,.T.);
#8825=EDGE_CURVE('',#7159,#7159,#6130,.T.);
#8826=EDGE_CURVE('',#7159,#7160,#4280,.T.);
#8827=EDGE_CURVE('',#7160,#7160,#6131,.T.);
#8828=EDGE_CURVE('',#7161,#7161,#6132,.T.);
#8829=EDGE_CURVE('',#7161,#7162,#4281,.T.);
#8830=EDGE_CURVE('',#7162,#7162,#6133,.T.);
#8831=EDGE_CURVE('',#7163,#7163,#6134,.T.);
#8832=EDGE_CURVE('',#7163,#7164,#4282,.T.);
#8833=EDGE_CURVE('',#7164,#7164,#6135,.T.);
#8834=EDGE_CURVE('',#7165,#7165,#6136,.T.);
#8835=EDGE_CURVE('',#7165,#7166,#4283,.T.);
#8836=EDGE_CURVE('',#7166,#7166,#6137,.T.);
#8837=EDGE_CURVE('',#7167,#7167,#6138,.T.);
#8838=EDGE_CURVE('',#7167,#7168,#4284,.T.);
#8839=EDGE_CURVE('',#7168,#7168,#6139,.T.);
#8840=EDGE_CURVE('',#7169,#7169,#6140,.T.);
#8841=EDGE_CURVE('',#7169,#7170,#4285,.T.);
#8842=EDGE_CURVE('',#7170,#7170,#6141,.T.);
#8843=EDGE_CURVE('',#7171,#7171,#6142,.T.);
#8844=EDGE_CURVE('',#7171,#7172,#4286,.T.);
#8845=EDGE_CURVE('',#7172,#7172,#6143,.T.);
#8846=EDGE_CURVE('',#7173,#7174,#4287,.T.);
#8847=EDGE_CURVE('',#7173,#7175,#4288,.T.);
#8848=EDGE_CURVE('',#7176,#7175,#4289,.T.);
#8849=EDGE_CURVE('',#7174,#7176,#4290,.T.);
#8850=EDGE_CURVE('',#7177,#7173,#4291,.T.);
#8851=EDGE_CURVE('',#7177,#7178,#4292,.T.);
#8852=EDGE_CURVE('',#7175,#7178,#4293,.T.);
#8853=EDGE_CURVE('',#7179,#7177,#4294,.T.);
#8854=EDGE_CURVE('',#7180,#7179,#4295,.T.);
#8855=EDGE_CURVE('',#7178,#7180,#4296,.T.);
#8856=EDGE_CURVE('',#7181,#7181,#6144,.T.);
#8857=EDGE_CURVE('',#7180,#7176,#6145,.T.);
#8858=EDGE_CURVE('',#7179,#7174,#6146,.T.);
#8859=EDGE_CURVE('',#7182,#7183,#4297,.T.);
#8860=EDGE_CURVE('',#7184,#7182,#6147,.T.);
#8861=EDGE_CURVE('',#7185,#7184,#4298,.T.);
#8862=EDGE_CURVE('',#7185,#7183,#6148,.T.);
#8863=EDGE_CURVE('',#7186,#7183,#4299,.T.);
#8864=EDGE_CURVE('',#7187,#7186,#4300,.T.);
#8865=EDGE_CURVE('',#7182,#7187,#4301,.T.);
#8866=EDGE_CURVE('',#7185,#7188,#4302,.T.);
#8867=EDGE_CURVE('',#7186,#7188,#6149,.T.);
#8868=EDGE_CURVE('',#7189,#7184,#4303,.T.);
#8869=EDGE_CURVE('',#7188,#7189,#4304,.T.);
#8870=EDGE_CURVE('',#7189,#7187,#6150,.T.);
#8871=EDGE_CURVE('',#7181,#7190,#4305,.T.);
#8872=EDGE_CURVE('',#7190,#7190,#6151,.T.);
#8873=EDGE_CURVE('',#7191,#7191,#6152,.T.);
#8874=EDGE_CURVE('',#7191,#7192,#4306,.T.);
#8875=EDGE_CURVE('',#7192,#7192,#6153,.T.);
#8876=EDGE_CURVE('',#7193,#7193,#6154,.T.);
#8877=EDGE_CURVE('',#7193,#7194,#4307,.T.);
#8878=EDGE_CURVE('',#7194,#7194,#6155,.T.);
#8879=EDGE_CURVE('',#7195,#7196,#4308,.T.);
#8880=EDGE_CURVE('',#7197,#7195,#4309,.T.);
#8881=EDGE_CURVE('',#7198,#7197,#4310,.T.);
#8882=EDGE_CURVE('',#7196,#7198,#4311,.T.);
#8883=EDGE_CURVE('',#7199,#7195,#4312,.T.);
#8884=EDGE_CURVE('',#7199,#7200,#4313,.T.);
#8885=EDGE_CURVE('',#7197,#7200,#4314,.T.);
#8886=EDGE_CURVE('',#7201,#7199,#4315,.T.);
#8887=EDGE_CURVE('',#7202,#7201,#4316,.T.);
#8888=EDGE_CURVE('',#7200,#7202,#4317,.T.);
#8889=EDGE_CURVE('',#7203,#7204,#6156,.T.);
#8890=EDGE_CURVE('',#7204,#7205,#51,.T.);
#8891=EDGE_CURVE('',#7205,#7206,#4318,.T.);
#8892=EDGE_CURVE('',#7206,#7207,#52,.T.);
#8893=EDGE_CURVE('',#7207,#7208,#6157,.T.);
#8894=EDGE_CURVE('',#7208,#7209,#53,.T.);
#8895=EDGE_CURVE('',#7209,#7210,#4319,.T.);
#8896=EDGE_CURVE('',#7210,#7211,#54,.T.);
#8897=EDGE_CURVE('',#7211,#7212,#6158,.T.);
#8898=EDGE_CURVE('',#7212,#7213,#55,.T.);
#8899=EDGE_CURVE('',#7213,#7214,#4320,.T.);
#8900=EDGE_CURVE('',#7214,#7215,#56,.T.);
#8901=EDGE_CURVE('',#7215,#7216,#6159,.T.);
#8902=EDGE_CURVE('',#7216,#7217,#57,.T.);
#8903=EDGE_CURVE('',#7217,#7218,#4321,.T.);
#8904=EDGE_CURVE('',#7218,#7219,#58,.T.);
#8905=EDGE_CURVE('',#7219,#7220,#6160,.T.);
#8906=EDGE_CURVE('',#7220,#7221,#59,.T.);
#8907=EDGE_CURVE('',#7221,#7222,#4322,.T.);
#8908=EDGE_CURVE('',#7222,#7223,#60,.T.);
#8909=EDGE_CURVE('',#7223,#7224,#6161,.T.);
#8910=EDGE_CURVE('',#7224,#7225,#61,.T.);
#8911=EDGE_CURVE('',#7225,#7226,#4323,.T.);
#8912=EDGE_CURVE('',#7226,#7227,#62,.T.);
#8913=EDGE_CURVE('',#7227,#7228,#6162,.T.);
#8914=EDGE_CURVE('',#7228,#7229,#63,.T.);
#8915=EDGE_CURVE('',#7229,#7230,#4324,.T.);
#8916=EDGE_CURVE('',#7230,#7231,#64,.T.);
#8917=EDGE_CURVE('',#7231,#7232,#6163,.T.);
#8918=EDGE_CURVE('',#7232,#7233,#65,.T.);
#8919=EDGE_CURVE('',#7233,#7234,#4325,.T.);
#8920=EDGE_CURVE('',#7234,#7235,#66,.T.);
#8921=EDGE_CURVE('',#7235,#7236,#6164,.T.);
#8922=EDGE_CURVE('',#7236,#7237,#67,.T.);
#8923=EDGE_CURVE('',#7237,#7238,#4326,.T.);
#8924=EDGE_CURVE('',#7238,#7239,#68,.T.);
#8925=EDGE_CURVE('',#7239,#7240,#6165,.T.);
#8926=EDGE_CURVE('',#7240,#7241,#69,.T.);
#8927=EDGE_CURVE('',#7241,#7242,#4327,.T.);
#8928=EDGE_CURVE('',#7242,#7243,#70,.T.);
#8929=EDGE_CURVE('',#7243,#7244,#6166,.T.);
#8930=EDGE_CURVE('',#7244,#7245,#71,.T.);
#8931=EDGE_CURVE('',#7245,#7246,#4328,.T.);
#8932=EDGE_CURVE('',#7246,#7247,#72,.T.);
#8933=EDGE_CURVE('',#7247,#7248,#6167,.T.);
#8934=EDGE_CURVE('',#7248,#7249,#73,.T.);
#8935=EDGE_CURVE('',#7249,#7250,#4329,.T.);
#8936=EDGE_CURVE('',#7250,#7251,#74,.T.);
#8937=EDGE_CURVE('',#7251,#7252,#6168,.T.);
#8938=EDGE_CURVE('',#7252,#7253,#75,.T.);
#8939=EDGE_CURVE('',#7253,#7254,#4330,.T.);
#8940=EDGE_CURVE('',#7254,#7255,#76,.T.);
#8941=EDGE_CURVE('',#7255,#7256,#6169,.T.);
#8942=EDGE_CURVE('',#7256,#7257,#77,.T.);
#8943=EDGE_CURVE('',#7257,#7258,#4331,.T.);
#8944=EDGE_CURVE('',#7258,#7259,#78,.T.);
#8945=EDGE_CURVE('',#7259,#7260,#6170,.T.);
#8946=EDGE_CURVE('',#7260,#7261,#79,.T.);
#8947=EDGE_CURVE('',#7261,#7262,#4332,.T.);
#8948=EDGE_CURVE('',#7262,#7263,#80,.T.);
#8949=EDGE_CURVE('',#7263,#7264,#6171,.T.);
#8950=EDGE_CURVE('',#7264,#7265,#81,.T.);
#8951=EDGE_CURVE('',#7265,#7266,#4333,.T.);
#8952=EDGE_CURVE('',#7266,#7267,#82,.T.);
#8953=EDGE_CURVE('',#7267,#7268,#6172,.T.);
#8954=EDGE_CURVE('',#7268,#7269,#83,.T.);
#8955=EDGE_CURVE('',#7269,#7270,#4334,.T.);
#8956=EDGE_CURVE('',#7270,#7271,#84,.T.);
#8957=EDGE_CURVE('',#7271,#7272,#6173,.T.);
#8958=EDGE_CURVE('',#7272,#7273,#85,.T.);
#8959=EDGE_CURVE('',#7273,#7274,#4335,.T.);
#8960=EDGE_CURVE('',#7274,#7275,#86,.T.);
#8961=EDGE_CURVE('',#7275,#7276,#6174,.T.);
#8962=EDGE_CURVE('',#7276,#7277,#87,.T.);
#8963=EDGE_CURVE('',#7277,#7278,#4336,.T.);
#8964=EDGE_CURVE('',#7278,#7279,#88,.T.);
#8965=EDGE_CURVE('',#7279,#7280,#6175,.T.);
#8966=EDGE_CURVE('',#7280,#7281,#89,.T.);
#8967=EDGE_CURVE('',#7281,#7282,#4337,.T.);
#8968=EDGE_CURVE('',#7282,#7203,#90,.T.);
#8969=EDGE_CURVE('',#7202,#7198,#6176,.T.);
#8970=EDGE_CURVE('',#7196,#7201,#6177,.T.);
#8971=EDGE_CURVE('',#7283,#7283,#6178,.T.);
#8972=EDGE_CURVE('',#7283,#7284,#4338,.T.);
#8973=EDGE_CURVE('',#7284,#7284,#6179,.T.);
#8974=EDGE_CURVE('',#7285,#7280,#4339,.T.);
#8975=EDGE_CURVE('',#7286,#7285,#91,.T.);
#8976=EDGE_CURVE('',#7281,#7286,#4340,.T.);
#8977=EDGE_CURVE('',#7287,#7286,#4341,.T.);
#8978=EDGE_CURVE('',#7282,#7287,#4342,.T.);
#8979=EDGE_CURVE('',#7288,#7287,#92,.T.);
#8980=EDGE_CURVE('',#7203,#7288,#4343,.T.);
#8981=EDGE_CURVE('',#7289,#7288,#6180,.T.);
#8982=EDGE_CURVE('',#7289,#7204,#4344,.T.);
#8983=EDGE_CURVE('',#7290,#7289,#93,.T.);
#8984=EDGE_CURVE('',#7205,#7290,#4345,.T.);
#8985=EDGE_CURVE('',#7291,#7290,#4346,.T.);
#8986=EDGE_CURVE('',#7206,#7291,#4347,.T.);
#8987=EDGE_CURVE('',#7292,#7291,#94,.T.);
#8988=EDGE_CURVE('',#7207,#7292,#4348,.T.);
#8989=EDGE_CURVE('',#7293,#7292,#6181,.T.);
#8990=EDGE_CURVE('',#7293,#7208,#4349,.T.);
#8991=EDGE_CURVE('',#7294,#7293,#95,.T.);
#8992=EDGE_CURVE('',#7209,#7294,#4350,.T.);
#8993=EDGE_CURVE('',#7295,#7294,#4351,.T.);
#8994=EDGE_CURVE('',#7210,#7295,#4352,.T.);
#8995=EDGE_CURVE('',#7296,#7295,#96,.T.);
#8996=EDGE_CURVE('',#7211,#7296,#4353,.T.);
#8997=EDGE_CURVE('',#7297,#7296,#6182,.T.);
#8998=EDGE_CURVE('',#7297,#7212,#4354,.T.);
#8999=EDGE_CURVE('',#7298,#7297,#97,.T.);
#9000=EDGE_CURVE('',#7213,#7298,#4355,.T.);
#9001=EDGE_CURVE('',#7299,#7298,#4356,.T.);
#9002=EDGE_CURVE('',#7214,#7299,#4357,.T.);
#9003=EDGE_CURVE('',#7300,#7299,#98,.T.);
#9004=EDGE_CURVE('',#7215,#7300,#4358,.T.);
#9005=EDGE_CURVE('',#7301,#7300,#6183,.T.);
#9006=EDGE_CURVE('',#7301,#7216,#4359,.T.);
#9007=EDGE_CURVE('',#7302,#7301,#99,.T.);
#9008=EDGE_CURVE('',#7217,#7302,#4360,.T.);
#9009=EDGE_CURVE('',#7303,#7302,#4361,.T.);
#9010=EDGE_CURVE('',#7218,#7303,#4362,.T.);
#9011=EDGE_CURVE('',#7304,#7303,#100,.T.);
#9012=EDGE_CURVE('',#7219,#7304,#4363,.T.);
#9013=EDGE_CURVE('',#7305,#7304,#6184,.T.);
#9014=EDGE_CURVE('',#7305,#7220,#4364,.T.);
#9015=EDGE_CURVE('',#7306,#7305,#101,.T.);
#9016=EDGE_CURVE('',#7221,#7306,#4365,.T.);
#9017=EDGE_CURVE('',#7307,#7306,#4366,.T.);
#9018=EDGE_CURVE('',#7222,#7307,#4367,.T.);
#9019=EDGE_CURVE('',#7308,#7307,#102,.T.);
#9020=EDGE_CURVE('',#7223,#7308,#4368,.T.);
#9021=EDGE_CURVE('',#7309,#7308,#6185,.T.);
#9022=EDGE_CURVE('',#7309,#7224,#4369,.T.);
#9023=EDGE_CURVE('',#7310,#7309,#103,.T.);
#9024=EDGE_CURVE('',#7225,#7310,#4370,.T.);
#9025=EDGE_CURVE('',#7311,#7310,#4371,.T.);
#9026=EDGE_CURVE('',#7226,#7311,#4372,.T.);
#9027=EDGE_CURVE('',#7312,#7311,#104,.T.);
#9028=EDGE_CURVE('',#7227,#7312,#4373,.T.);
#9029=EDGE_CURVE('',#7313,#7312,#6186,.T.);
#9030=EDGE_CURVE('',#7313,#7228,#4374,.T.);
#9031=EDGE_CURVE('',#7314,#7313,#105,.T.);
#9032=EDGE_CURVE('',#7229,#7314,#4375,.T.);
#9033=EDGE_CURVE('',#7315,#7314,#4376,.T.);
#9034=EDGE_CURVE('',#7230,#7315,#4377,.T.);
#9035=EDGE_CURVE('',#7316,#7315,#106,.T.);
#9036=EDGE_CURVE('',#7231,#7316,#4378,.T.);
#9037=EDGE_CURVE('',#7317,#7316,#6187,.T.);
#9038=EDGE_CURVE('',#7317,#7232,#4379,.T.);
#9039=EDGE_CURVE('',#7318,#7317,#107,.T.);
#9040=EDGE_CURVE('',#7233,#7318,#4380,.T.);
#9041=EDGE_CURVE('',#7319,#7318,#4381,.T.);
#9042=EDGE_CURVE('',#7234,#7319,#4382,.T.);
#9043=EDGE_CURVE('',#7320,#7319,#108,.T.);
#9044=EDGE_CURVE('',#7235,#7320,#4383,.T.);
#9045=EDGE_CURVE('',#7321,#7320,#6188,.T.);
#9046=EDGE_CURVE('',#7321,#7236,#4384,.T.);
#9047=EDGE_CURVE('',#7322,#7321,#109,.T.);
#9048=EDGE_CURVE('',#7237,#7322,#4385,.T.);
#9049=EDGE_CURVE('',#7323,#7322,#4386,.T.);
#9050=EDGE_CURVE('',#7238,#7323,#4387,.T.);
#9051=EDGE_CURVE('',#7324,#7323,#110,.T.);
#9052=EDGE_CURVE('',#7239,#7324,#4388,.T.);
#9053=EDGE_CURVE('',#7325,#7324,#6189,.T.);
#9054=EDGE_CURVE('',#7325,#7240,#4389,.T.);
#9055=EDGE_CURVE('',#7326,#7325,#111,.T.);
#9056=EDGE_CURVE('',#7241,#7326,#4390,.T.);
#9057=EDGE_CURVE('',#7327,#7326,#4391,.T.);
#9058=EDGE_CURVE('',#7242,#7327,#4392,.T.);
#9059=EDGE_CURVE('',#7328,#7327,#112,.T.);
#9060=EDGE_CURVE('',#7243,#7328,#4393,.T.);
#9061=EDGE_CURVE('',#7329,#7328,#6190,.T.);
#9062=EDGE_CURVE('',#7329,#7244,#4394,.T.);
#9063=EDGE_CURVE('',#7330,#7329,#113,.T.);
#9064=EDGE_CURVE('',#7245,#7330,#4395,.T.);
#9065=EDGE_CURVE('',#7331,#7330,#4396,.T.);
#9066=EDGE_CURVE('',#7246,#7331,#4397,.T.);
#9067=EDGE_CURVE('',#7332,#7331,#114,.T.);
#9068=EDGE_CURVE('',#7247,#7332,#4398,.T.);
#9069=EDGE_CURVE('',#7333,#7332,#6191,.T.);
#9070=EDGE_CURVE('',#7333,#7248,#4399,.T.);
#9071=EDGE_CURVE('',#7334,#7333,#115,.T.);
#9072=EDGE_CURVE('',#7249,#7334,#4400,.T.);
#9073=EDGE_CURVE('',#7335,#7334,#4401,.T.);
#9074=EDGE_CURVE('',#7250,#7335,#4402,.T.);
#9075=EDGE_CURVE('',#7336,#7335,#116,.T.);
#9076=EDGE_CURVE('',#7251,#7336,#4403,.T.);
#9077=EDGE_CURVE('',#7337,#7336,#6192,.T.);
#9078=EDGE_CURVE('',#7337,#7252,#4404,.T.);
#9079=EDGE_CURVE('',#7338,#7337,#117,.T.);
#9080=EDGE_CURVE('',#7253,#7338,#4405,.T.);
#9081=EDGE_CURVE('',#7339,#7338,#4406,.T.);
#9082=EDGE_CURVE('',#7254,#7339,#4407,.T.);
#9083=EDGE_CURVE('',#7340,#7339,#118,.T.);
#9084=EDGE_CURVE('',#7255,#7340,#4408,.T.);
#9085=EDGE_CURVE('',#7341,#7340,#6193,.T.);
#9086=EDGE_CURVE('',#7341,#7256,#4409,.T.);
#9087=EDGE_CURVE('',#7342,#7341,#119,.T.);
#9088=EDGE_CURVE('',#7257,#7342,#4410,.T.);
#9089=EDGE_CURVE('',#7343,#7342,#4411,.T.);
#9090=EDGE_CURVE('',#7258,#7343,#4412,.T.);
#9091=EDGE_CURVE('',#7344,#7343,#120,.T.);
#9092=EDGE_CURVE('',#7259,#7344,#4413,.T.);
#9093=EDGE_CURVE('',#7345,#7344,#6194,.T.);
#9094=EDGE_CURVE('',#7345,#7260,#4414,.T.);
#9095=EDGE_CURVE('',#7346,#7345,#121,.T.);
#9096=EDGE_CURVE('',#7261,#7346,#4415,.T.);
#9097=EDGE_CURVE('',#7347,#7346,#4416,.T.);
#9098=EDGE_CURVE('',#7262,#7347,#4417,.T.);
#9099=EDGE_CURVE('',#7348,#7347,#122,.T.);
#9100=EDGE_CURVE('',#7263,#7348,#4418,.T.);
#9101=EDGE_CURVE('',#7349,#7348,#6195,.T.);
#9102=EDGE_CURVE('',#7349,#7264,#4419,.T.);
#9103=EDGE_CURVE('',#7350,#7349,#123,.T.);
#9104=EDGE_CURVE('',#7265,#7350,#4420,.T.);
#9105=EDGE_CURVE('',#7351,#7350,#4421,.T.);
#9106=EDGE_CURVE('',#7266,#7351,#4422,.T.);
#9107=EDGE_CURVE('',#7352,#7351,#124,.T.);
#9108=EDGE_CURVE('',#7267,#7352,#4423,.T.);
#9109=EDGE_CURVE('',#7353,#7352,#6196,.T.);
#9110=EDGE_CURVE('',#7353,#7268,#4424,.T.);
#9111=EDGE_CURVE('',#7354,#7353,#125,.T.);
#9112=EDGE_CURVE('',#7269,#7354,#4425,.T.);
#9113=EDGE_CURVE('',#7355,#7354,#4426,.T.);
#9114=EDGE_CURVE('',#7270,#7355,#4427,.T.);
#9115=EDGE_CURVE('',#7356,#7355,#126,.T.);
#9116=EDGE_CURVE('',#7271,#7356,#4428,.T.);
#9117=EDGE_CURVE('',#7357,#7356,#6197,.T.);
#9118=EDGE_CURVE('',#7357,#7272,#4429,.T.);
#9119=EDGE_CURVE('',#7358,#7357,#127,.T.);
#9120=EDGE_CURVE('',#7273,#7358,#4430,.T.);
#9121=EDGE_CURVE('',#7359,#7358,#4431,.T.);
#9122=EDGE_CURVE('',#7274,#7359,#4432,.T.);
#9123=EDGE_CURVE('',#7360,#7359,#128,.T.);
#9124=EDGE_CURVE('',#7275,#7360,#4433,.T.);
#9125=EDGE_CURVE('',#7361,#7360,#6198,.T.);
#9126=EDGE_CURVE('',#7361,#7276,#4434,.T.);
#9127=EDGE_CURVE('',#7362,#7361,#129,.T.);
#9128=EDGE_CURVE('',#7277,#7362,#4435,.T.);
#9129=EDGE_CURVE('',#7363,#7362,#4436,.T.);
#9130=EDGE_CURVE('',#7278,#7363,#4437,.T.);
#9131=EDGE_CURVE('',#7364,#7363,#130,.T.);
#9132=EDGE_CURVE('',#7279,#7364,#4438,.T.);
#9133=EDGE_CURVE('',#7285,#7364,#6199,.T.);
#9134=EDGE_CURVE('',#7365,#7365,#6200,.T.);
#9135=EDGE_CURVE('',#7366,#7366,#6201,.T.);
#9136=EDGE_CURVE('',#7366,#7365,#4439,.T.);
#9137=EDGE_CURVE('',#7367,#7367,#6202,.T.);
#9138=EDGE_CURVE('',#7367,#7366,#4440,.T.);
#9139=EDGE_CURVE('',#7368,#7368,#6203,.T.);
#9140=EDGE_CURVE('',#7368,#7367,#4441,.T.);
#9141=EDGE_CURVE('',#7369,#7369,#6204,.T.);
#9142=EDGE_CURVE('',#7370,#7370,#6205,.F.);
#9143=EDGE_CURVE('',#7370,#7369,#4442,.T.);
#9144=EDGE_CURVE('',#7371,#7371,#6206,.F.);
#9145=EDGE_CURVE('',#7371,#7370,#4443,.T.);
#9146=EDGE_CURVE('',#7372,#7372,#6207,.T.);
#9147=EDGE_CURVE('',#7372,#7371,#4444,.T.);
#9148=EDGE_CURVE('',#7373,#7374,#4445,.T.);
#9149=EDGE_CURVE('',#7374,#7375,#4446,.T.);
#9150=EDGE_CURVE('',#7375,#7376,#4447,.T.);
#9151=EDGE_CURVE('',#7373,#7376,#4448,.T.);
#9152=EDGE_CURVE('',#7374,#7377,#4449,.T.);
#9153=EDGE_CURVE('',#7377,#7378,#4450,.T.);
#9154=EDGE_CURVE('',#7378,#7375,#4451,.T.);
#9155=EDGE_CURVE('',#7377,#7379,#4452,.T.);
#9156=EDGE_CURVE('',#7379,#7380,#4453,.T.);
#9157=EDGE_CURVE('',#7380,#7378,#4454,.T.);
#9158=EDGE_CURVE('',#7379,#7381,#4455,.T.);
#9159=EDGE_CURVE('',#7381,#7382,#4456,.T.);
#9160=EDGE_CURVE('',#7382,#7380,#4457,.T.);
#9161=EDGE_CURVE('',#7381,#7383,#4458,.T.);
#9162=EDGE_CURVE('',#7383,#7384,#4459,.T.);
#9163=EDGE_CURVE('',#7384,#7382,#4460,.T.);
#9164=EDGE_CURVE('',#7383,#7373,#4461,.T.);
#9165=EDGE_CURVE('',#7376,#7384,#4462,.T.);
#9166=EDGE_CURVE('',#7385,#7386,#4463,.T.);
#9167=EDGE_CURVE('',#7387,#7385,#4464,.T.);
#9168=EDGE_CURVE('',#7388,#7387,#4465,.T.);
#9169=EDGE_CURVE('',#7389,#7388,#4466,.T.);
#9170=EDGE_CURVE('',#7390,#7389,#4467,.T.);
#9171=EDGE_CURVE('',#7391,#7390,#4468,.T.);
#9172=EDGE_CURVE('',#7392,#7391,#4469,.T.);
#9173=EDGE_CURVE('',#7386,#7392,#4470,.T.);
#9174=EDGE_CURVE('',#7389,#7393,#4471,.T.);
#9175=EDGE_CURVE('',#7393,#7394,#4472,.T.);
#9176=EDGE_CURVE('',#7394,#7390,#4473,.T.);
#9177=EDGE_CURVE('',#7395,#7388,#4474,.T.);
#9178=EDGE_CURVE('',#7395,#7393,#4475,.T.);
#9179=EDGE_CURVE('',#7387,#7396,#4476,.T.);
#9180=EDGE_CURVE('',#7396,#7395,#4477,.T.);
#9181=EDGE_CURVE('',#7397,#7385,#4478,.T.);
#9182=EDGE_CURVE('',#7397,#7396,#4479,.T.);
#9183=EDGE_CURVE('',#7398,#7397,#4480,.T.);
#9184=EDGE_CURVE('',#7399,#7398,#4481,.T.);
#9185=EDGE_CURVE('',#7400,#7399,#4482,.T.);
#9186=EDGE_CURVE('',#7394,#7400,#4483,.T.);
#9187=EDGE_CURVE('',#7386,#7398,#4484,.T.);
#9188=EDGE_CURVE('',#7399,#7392,#4485,.T.);
#9189=EDGE_CURVE('',#7391,#7400,#4486,.T.);
#9190=EDGE_CURVE('',#7401,#7401,#6208,.T.);
#9191=EDGE_CURVE('',#7401,#7402,#4487,.T.);
#9192=EDGE_CURVE('',#7402,#7402,#6209,.T.);
#9193=EDGE_CURVE('',#7403,#7403,#6210,.T.);
#9194=EDGE_CURVE('',#7403,#7404,#4488,.T.);
#9195=EDGE_CURVE('',#7404,#7404,#6211,.T.);
#9196=EDGE_CURVE('',#7405,#7405,#6212,.T.);
#9197=EDGE_CURVE('',#7406,#7406,#6213,.T.);
#9198=EDGE_CURVE('',#7406,#7405,#4489,.T.);
#9199=EDGE_CURVE('',#7407,#7407,#6214,.T.);
#9200=EDGE_CURVE('',#7407,#7406,#4490,.T.);
#9201=EDGE_CURVE('',#7408,#7408,#6215,.T.);
#9202=EDGE_CURVE('',#7408,#7407,#4491,.T.);
#9203=EDGE_CURVE('',#7409,#7409,#6216,.T.);
#9204=EDGE_CURVE('',#7410,#7410,#6217,.F.);
#9205=EDGE_CURVE('',#7410,#7409,#4492,.T.);
#9206=EDGE_CURVE('',#7411,#7411,#6218,.F.);
#9207=EDGE_CURVE('',#7411,#7410,#4493,.T.);
#9208=EDGE_CURVE('',#7412,#7412,#6219,.T.);
#9209=EDGE_CURVE('',#7412,#7411,#4494,.T.);
#9210=EDGE_CURVE('',#7413,#7414,#4495,.T.);
#9211=EDGE_CURVE('',#7414,#7415,#4496,.T.);
#9212=EDGE_CURVE('',#7415,#7416,#4497,.T.);
#9213=EDGE_CURVE('',#7413,#7416,#4498,.T.);
#9214=EDGE_CURVE('',#7414,#7417,#4499,.T.);
#9215=EDGE_CURVE('',#7417,#7418,#4500,.T.);
#9216=EDGE_CURVE('',#7418,#7415,#4501,.T.);
#9217=EDGE_CURVE('',#7417,#7419,#4502,.T.);
#9218=EDGE_CURVE('',#7419,#7420,#4503,.T.);
#9219=EDGE_CURVE('',#7420,#7418,#4504,.T.);
#9220=EDGE_CURVE('',#7419,#7421,#4505,.T.);
#9221=EDGE_CURVE('',#7421,#7422,#4506,.T.);
#9222=EDGE_CURVE('',#7422,#7420,#4507,.T.);
#9223=EDGE_CURVE('',#7421,#7423,#4508,.T.);
#9224=EDGE_CURVE('',#7423,#7424,#4509,.T.);
#9225=EDGE_CURVE('',#7424,#7422,#4510,.T.);
#9226=EDGE_CURVE('',#7423,#7413,#4511,.T.);
#9227=EDGE_CURVE('',#7416,#7424,#4512,.T.);
#9228=EDGE_CURVE('',#7425,#7425,#6220,.T.);
#9229=EDGE_CURVE('',#7425,#7426,#4513,.T.);
#9230=EDGE_CURVE('',#7426,#7426,#6221,.T.);
#9231=EDGE_CURVE('',#7427,#7427,#6222,.T.);
#9232=EDGE_CURVE('',#7427,#7428,#4514,.T.);
#9233=EDGE_CURVE('',#7428,#7428,#6223,.T.);
#9234=ORIENTED_EDGE('',*,*,#7429,.F.);
#9235=ORIENTED_EDGE('',*,*,#7430,.T.);
#9236=ORIENTED_EDGE('',*,*,#7431,.F.);
#9237=ORIENTED_EDGE('',*,*,#7430,.F.);
#9238=ORIENTED_EDGE('',*,*,#7432,.F.);
#9239=ORIENTED_EDGE('',*,*,#7433,.T.);
#9240=ORIENTED_EDGE('',*,*,#7434,.F.);
#9241=ORIENTED_EDGE('',*,*,#7433,.F.);
#9242=ORIENTED_EDGE('',*,*,#7435,.F.);
#9243=ORIENTED_EDGE('',*,*,#7436,.T.);
#9244=ORIENTED_EDGE('',*,*,#7437,.F.);
#9245=ORIENTED_EDGE('',*,*,#7436,.F.);
#9246=ORIENTED_EDGE('',*,*,#7438,.F.);
#9247=ORIENTED_EDGE('',*,*,#7439,.T.);
#9248=ORIENTED_EDGE('',*,*,#7440,.F.);
#9249=ORIENTED_EDGE('',*,*,#7439,.F.);
#9250=ORIENTED_EDGE('',*,*,#7441,.T.);
#9251=ORIENTED_EDGE('',*,*,#7442,.T.);
#9252=ORIENTED_EDGE('',*,*,#7443,.F.);
#9253=ORIENTED_EDGE('',*,*,#7444,.F.);
#9254=ORIENTED_EDGE('',*,*,#7445,.T.);
#9255=ORIENTED_EDGE('',*,*,#7444,.T.);
#9256=ORIENTED_EDGE('',*,*,#7446,.F.);
#9257=ORIENTED_EDGE('',*,*,#7447,.F.);
#9258=ORIENTED_EDGE('',*,*,#7448,.T.);
#9259=ORIENTED_EDGE('',*,*,#7447,.T.);
#9260=ORIENTED_EDGE('',*,*,#7449,.F.);
#9261=ORIENTED_EDGE('',*,*,#7450,.F.);
#9262=ORIENTED_EDGE('',*,*,#7451,.T.);
#9263=ORIENTED_EDGE('',*,*,#7450,.T.);
#9264=ORIENTED_EDGE('',*,*,#7452,.F.);
#9265=ORIENTED_EDGE('',*,*,#7442,.F.);
#9266=ORIENTED_EDGE('',*,*,#7452,.T.);
#9267=ORIENTED_EDGE('',*,*,#7449,.T.);
#9268=ORIENTED_EDGE('',*,*,#7446,.T.);
#9269=ORIENTED_EDGE('',*,*,#7443,.T.);
#9270=ORIENTED_EDGE('',*,*,#7431,.T.);
#9271=ORIENTED_EDGE('',*,*,#7434,.T.);
#9272=ORIENTED_EDGE('',*,*,#7437,.T.);
#9273=ORIENTED_EDGE('',*,*,#7440,.T.);
#9274=ORIENTED_EDGE('',*,*,#7451,.F.);
#9275=ORIENTED_EDGE('',*,*,#7441,.F.);
#9276=ORIENTED_EDGE('',*,*,#7445,.F.);
#9277=ORIENTED_EDGE('',*,*,#7448,.F.);
#9278=ORIENTED_EDGE('',*,*,#7429,.T.);
#9279=ORIENTED_EDGE('',*,*,#7432,.T.);
#9280=ORIENTED_EDGE('',*,*,#7435,.T.);
#9281=ORIENTED_EDGE('',*,*,#7438,.T.);
#9282=ORIENTED_EDGE('',*,*,#7453,.T.);
#9283=ORIENTED_EDGE('',*,*,#7454,.T.);
#9284=ORIENTED_EDGE('',*,*,#7455,.F.);
#9285=ORIENTED_EDGE('',*,*,#7456,.F.);
#9286=ORIENTED_EDGE('',*,*,#7457,.T.);
#9287=ORIENTED_EDGE('',*,*,#7456,.T.);
#9288=ORIENTED_EDGE('',*,*,#7458,.F.);
#9289=ORIENTED_EDGE('',*,*,#7459,.F.);
#9290=ORIENTED_EDGE('',*,*,#7460,.T.);
#9291=ORIENTED_EDGE('',*,*,#7459,.T.);
#9292=ORIENTED_EDGE('',*,*,#7461,.F.);
#9293=ORIENTED_EDGE('',*,*,#7462,.F.);
#9294=ORIENTED_EDGE('',*,*,#7463,.T.);
#9295=ORIENTED_EDGE('',*,*,#7462,.T.);
#9296=ORIENTED_EDGE('',*,*,#7464,.F.);
#9297=ORIENTED_EDGE('',*,*,#7454,.F.);
#9298=ORIENTED_EDGE('',*,*,#7464,.T.);
#9299=ORIENTED_EDGE('',*,*,#7461,.T.);
#9300=ORIENTED_EDGE('',*,*,#7458,.T.);
#9301=ORIENTED_EDGE('',*,*,#7455,.T.);
#9302=ORIENTED_EDGE('',*,*,#7463,.F.);
#9303=ORIENTED_EDGE('',*,*,#7453,.F.);
#9304=ORIENTED_EDGE('',*,*,#7457,.F.);
#9305=ORIENTED_EDGE('',*,*,#7460,.F.);
#9306=ORIENTED_EDGE('',*,*,#7465,.T.);
#9307=ORIENTED_EDGE('',*,*,#7466,.T.);
#9308=ORIENTED_EDGE('',*,*,#7467,.F.);
#9309=ORIENTED_EDGE('',*,*,#7468,.F.);
#9310=ORIENTED_EDGE('',*,*,#7469,.T.);
#9311=ORIENTED_EDGE('',*,*,#7468,.T.);
#9312=ORIENTED_EDGE('',*,*,#7470,.F.);
#9313=ORIENTED_EDGE('',*,*,#7471,.F.);
#9314=ORIENTED_EDGE('',*,*,#7472,.T.);
#9315=ORIENTED_EDGE('',*,*,#7471,.T.);
#9316=ORIENTED_EDGE('',*,*,#7473,.F.);
#9317=ORIENTED_EDGE('',*,*,#7474,.F.);
#9318=ORIENTED_EDGE('',*,*,#7475,.T.);
#9319=ORIENTED_EDGE('',*,*,#7474,.T.);
#9320=ORIENTED_EDGE('',*,*,#7476,.F.);
#9321=ORIENTED_EDGE('',*,*,#7466,.F.);
#9322=ORIENTED_EDGE('',*,*,#7476,.T.);
#9323=ORIENTED_EDGE('',*,*,#7473,.T.);
#9324=ORIENTED_EDGE('',*,*,#7470,.T.);
#9325=ORIENTED_EDGE('',*,*,#7467,.T.);
#9326=ORIENTED_EDGE('',*,*,#7475,.F.);
#9327=ORIENTED_EDGE('',*,*,#7465,.F.);
#9328=ORIENTED_EDGE('',*,*,#7469,.F.);
#9329=ORIENTED_EDGE('',*,*,#7472,.F.);
#9330=ORIENTED_EDGE('',*,*,#7477,.F.);
#9331=ORIENTED_EDGE('',*,*,#7478,.T.);
#9332=ORIENTED_EDGE('',*,*,#7479,.F.);
#9333=ORIENTED_EDGE('',*,*,#7478,.F.);
#9334=ORIENTED_EDGE('',*,*,#7480,.F.);
#9335=ORIENTED_EDGE('',*,*,#7481,.T.);
#9336=ORIENTED_EDGE('',*,*,#7482,.F.);
#9337=ORIENTED_EDGE('',*,*,#7481,.F.);
#9338=ORIENTED_EDGE('',*,*,#7483,.F.);
#9339=ORIENTED_EDGE('',*,*,#7484,.T.);
#9340=ORIENTED_EDGE('',*,*,#7485,.F.);
#9341=ORIENTED_EDGE('',*,*,#7484,.F.);
#9342=ORIENTED_EDGE('',*,*,#7486,.F.);
#9343=ORIENTED_EDGE('',*,*,#7487,.T.);
#9344=ORIENTED_EDGE('',*,*,#7488,.F.);
#9345=ORIENTED_EDGE('',*,*,#7487,.F.);
#9346=ORIENTED_EDGE('',*,*,#7489,.F.);
#9347=ORIENTED_EDGE('',*,*,#7490,.T.);
#9348=ORIENTED_EDGE('',*,*,#7491,.F.);
#9349=ORIENTED_EDGE('',*,*,#7490,.F.);
#9350=ORIENTED_EDGE('',*,*,#7492,.F.);
#9351=ORIENTED_EDGE('',*,*,#7493,.T.);
#9352=ORIENTED_EDGE('',*,*,#7494,.F.);
#9353=ORIENTED_EDGE('',*,*,#7493,.F.);
#9354=ORIENTED_EDGE('',*,*,#7495,.F.);
#9355=ORIENTED_EDGE('',*,*,#7496,.T.);
#9356=ORIENTED_EDGE('',*,*,#7497,.F.);
#9357=ORIENTED_EDGE('',*,*,#7496,.F.);
#9358=ORIENTED_EDGE('',*,*,#7498,.F.);
#9359=ORIENTED_EDGE('',*,*,#7499,.T.);
#9360=ORIENTED_EDGE('',*,*,#7500,.F.);
#9361=ORIENTED_EDGE('',*,*,#7499,.F.);
#9362=ORIENTED_EDGE('',*,*,#7501,.F.);
#9363=ORIENTED_EDGE('',*,*,#7502,.T.);
#9364=ORIENTED_EDGE('',*,*,#7503,.F.);
#9365=ORIENTED_EDGE('',*,*,#7502,.F.);
#9366=ORIENTED_EDGE('',*,*,#7504,.F.);
#9367=ORIENTED_EDGE('',*,*,#7505,.T.);
#9368=ORIENTED_EDGE('',*,*,#7506,.F.);
#9369=ORIENTED_EDGE('',*,*,#7505,.F.);
#9370=ORIENTED_EDGE('',*,*,#7507,.F.);
#9371=ORIENTED_EDGE('',*,*,#7508,.T.);
#9372=ORIENTED_EDGE('',*,*,#7509,.F.);
#9373=ORIENTED_EDGE('',*,*,#7508,.F.);
#9374=ORIENTED_EDGE('',*,*,#7510,.F.);
#9375=ORIENTED_EDGE('',*,*,#7511,.T.);
#9376=ORIENTED_EDGE('',*,*,#7512,.F.);
#9377=ORIENTED_EDGE('',*,*,#7511,.F.);
#9378=ORIENTED_EDGE('',*,*,#7513,.F.);
#9379=ORIENTED_EDGE('',*,*,#7514,.T.);
#9380=ORIENTED_EDGE('',*,*,#7515,.F.);
#9381=ORIENTED_EDGE('',*,*,#7514,.F.);
#9382=ORIENTED_EDGE('',*,*,#7516,.F.);
#9383=ORIENTED_EDGE('',*,*,#7517,.T.);
#9384=ORIENTED_EDGE('',*,*,#7518,.F.);
#9385=ORIENTED_EDGE('',*,*,#7517,.F.);
#9386=ORIENTED_EDGE('',*,*,#7519,.F.);
#9387=ORIENTED_EDGE('',*,*,#7520,.T.);
#9388=ORIENTED_EDGE('',*,*,#7521,.F.);
#9389=ORIENTED_EDGE('',*,*,#7520,.F.);
#9390=ORIENTED_EDGE('',*,*,#7522,.F.);
#9391=ORIENTED_EDGE('',*,*,#7523,.T.);
#9392=ORIENTED_EDGE('',*,*,#7524,.F.);
#9393=ORIENTED_EDGE('',*,*,#7523,.F.);
#9394=ORIENTED_EDGE('',*,*,#7525,.T.);
#9395=ORIENTED_EDGE('',*,*,#7526,.T.);
#9396=ORIENTED_EDGE('',*,*,#7527,.F.);
#9397=ORIENTED_EDGE('',*,*,#7528,.F.);
#9398=ORIENTED_EDGE('',*,*,#7529,.T.);
#9399=ORIENTED_EDGE('',*,*,#7528,.T.);
#9400=ORIENTED_EDGE('',*,*,#7530,.F.);
#9401=ORIENTED_EDGE('',*,*,#7531,.F.);
#9402=ORIENTED_EDGE('',*,*,#7532,.T.);
#9403=ORIENTED_EDGE('',*,*,#7531,.T.);
#9404=ORIENTED_EDGE('',*,*,#7533,.F.);
#9405=ORIENTED_EDGE('',*,*,#7534,.F.);
#9406=ORIENTED_EDGE('',*,*,#7535,.T.);
#9407=ORIENTED_EDGE('',*,*,#7534,.T.);
#9408=ORIENTED_EDGE('',*,*,#7536,.F.);
#9409=ORIENTED_EDGE('',*,*,#7526,.F.);
#9410=ORIENTED_EDGE('',*,*,#7536,.T.);
#9411=ORIENTED_EDGE('',*,*,#7533,.T.);
#9412=ORIENTED_EDGE('',*,*,#7530,.T.);
#9413=ORIENTED_EDGE('',*,*,#7527,.T.);
#9414=ORIENTED_EDGE('',*,*,#7485,.T.);
#9415=ORIENTED_EDGE('',*,*,#7488,.T.);
#9416=ORIENTED_EDGE('',*,*,#7497,.T.);
#9417=ORIENTED_EDGE('',*,*,#7500,.T.);
#9418=ORIENTED_EDGE('',*,*,#7524,.T.);
#9419=ORIENTED_EDGE('',*,*,#7521,.T.);
#9420=ORIENTED_EDGE('',*,*,#7518,.T.);
#9421=ORIENTED_EDGE('',*,*,#7515,.T.);
#9422=ORIENTED_EDGE('',*,*,#7512,.T.);
#9423=ORIENTED_EDGE('',*,*,#7509,.T.);
#9424=ORIENTED_EDGE('',*,*,#7506,.T.);
#9425=ORIENTED_EDGE('',*,*,#7503,.T.);
#9426=ORIENTED_EDGE('',*,*,#7494,.T.);
#9427=ORIENTED_EDGE('',*,*,#7491,.T.);
#9428=ORIENTED_EDGE('',*,*,#7482,.T.);
#9429=ORIENTED_EDGE('',*,*,#7479,.T.);
#9430=ORIENTED_EDGE('',*,*,#7535,.F.);
#9431=ORIENTED_EDGE('',*,*,#7525,.F.);
#9432=ORIENTED_EDGE('',*,*,#7529,.F.);
#9433=ORIENTED_EDGE('',*,*,#7532,.F.);
#9434=ORIENTED_EDGE('',*,*,#7483,.T.);
#9435=ORIENTED_EDGE('',*,*,#7486,.T.);
#9436=ORIENTED_EDGE('',*,*,#7495,.T.);
#9437=ORIENTED_EDGE('',*,*,#7498,.T.);
#9438=ORIENTED_EDGE('',*,*,#7522,.T.);
#9439=ORIENTED_EDGE('',*,*,#7519,.T.);
#9440=ORIENTED_EDGE('',*,*,#7516,.T.);
#9441=ORIENTED_EDGE('',*,*,#7513,.T.);
#9442=ORIENTED_EDGE('',*,*,#7510,.T.);
#9443=ORIENTED_EDGE('',*,*,#7507,.T.);
#9444=ORIENTED_EDGE('',*,*,#7504,.T.);
#9445=ORIENTED_EDGE('',*,*,#7501,.T.);
#9446=ORIENTED_EDGE('',*,*,#7492,.T.);
#9447=ORIENTED_EDGE('',*,*,#7489,.T.);
#9448=ORIENTED_EDGE('',*,*,#7480,.T.);
#9449=ORIENTED_EDGE('',*,*,#7477,.T.);
#9450=ORIENTED_EDGE('',*,*,#7537,.F.);
#9451=ORIENTED_EDGE('',*,*,#7538,.T.);
#9452=ORIENTED_EDGE('',*,*,#7539,.F.);
#9453=ORIENTED_EDGE('',*,*,#7538,.F.);
#9454=ORIENTED_EDGE('',*,*,#7537,.T.);
#9455=ORIENTED_EDGE('',*,*,#7540,.F.);
#9456=ORIENTED_EDGE('',*,*,#7541,.F.);
#9457=ORIENTED_EDGE('',*,*,#7542,.T.);
#9458=ORIENTED_EDGE('',*,*,#7543,.F.);
#9459=ORIENTED_EDGE('',*,*,#7542,.F.);
#9460=ORIENTED_EDGE('',*,*,#7541,.T.);
#9461=ORIENTED_EDGE('',*,*,#7544,.F.);
#9462=ORIENTED_EDGE('',*,*,#7545,.F.);
#9463=ORIENTED_EDGE('',*,*,#7546,.T.);
#9464=ORIENTED_EDGE('',*,*,#7540,.T.);
#9465=ORIENTED_EDGE('',*,*,#7546,.F.);
#9466=ORIENTED_EDGE('',*,*,#7547,.F.);
#9467=ORIENTED_EDGE('',*,*,#7548,.T.);
#9468=ORIENTED_EDGE('',*,*,#7544,.T.);
#9469=ORIENTED_EDGE('',*,*,#7548,.F.);
#9470=ORIENTED_EDGE('',*,*,#7549,.T.);
#9471=ORIENTED_EDGE('',*,*,#7550,.T.);
#9472=ORIENTED_EDGE('',*,*,#7551,.F.);
#9473=ORIENTED_EDGE('',*,*,#7552,.F.);
#9474=ORIENTED_EDGE('',*,*,#7553,.T.);
#9475=ORIENTED_EDGE('',*,*,#7552,.T.);
#9476=ORIENTED_EDGE('',*,*,#7554,.F.);
#9477=ORIENTED_EDGE('',*,*,#7555,.F.);
#9478=ORIENTED_EDGE('',*,*,#7556,.T.);
#9479=ORIENTED_EDGE('',*,*,#7555,.T.);
#9480=ORIENTED_EDGE('',*,*,#7557,.F.);
#9481=ORIENTED_EDGE('',*,*,#7558,.F.);
#9482=ORIENTED_EDGE('',*,*,#7559,.T.);
#9483=ORIENTED_EDGE('',*,*,#7558,.T.);
#9484=ORIENTED_EDGE('',*,*,#7560,.F.);
#9485=ORIENTED_EDGE('',*,*,#7550,.F.);
#9486=ORIENTED_EDGE('',*,*,#7560,.T.);
#9487=ORIENTED_EDGE('',*,*,#7557,.T.);
#9488=ORIENTED_EDGE('',*,*,#7554,.T.);
#9489=ORIENTED_EDGE('',*,*,#7551,.T.);
#9490=ORIENTED_EDGE('',*,*,#7539,.T.);
#9491=ORIENTED_EDGE('',*,*,#7543,.T.);
#9492=ORIENTED_EDGE('',*,*,#7559,.F.);
#9493=ORIENTED_EDGE('',*,*,#7549,.F.);
#9494=ORIENTED_EDGE('',*,*,#7553,.F.);
#9495=ORIENTED_EDGE('',*,*,#7556,.F.);
#9496=ORIENTED_EDGE('',*,*,#7545,.T.);
#9497=ORIENTED_EDGE('',*,*,#7547,.T.);
#9498=ORIENTED_EDGE('',*,*,#7561,.T.);
#9499=ORIENTED_EDGE('',*,*,#7562,.T.);
#9500=ORIENTED_EDGE('',*,*,#7563,.F.);
#9501=ORIENTED_EDGE('',*,*,#7564,.F.);
#9502=ORIENTED_EDGE('',*,*,#7565,.T.);
#9503=ORIENTED_EDGE('',*,*,#7564,.T.);
#9504=ORIENTED_EDGE('',*,*,#7566,.F.);
#9505=ORIENTED_EDGE('',*,*,#7567,.F.);
#9506=ORIENTED_EDGE('',*,*,#7568,.T.);
#9507=ORIENTED_EDGE('',*,*,#7567,.T.);
#9508=ORIENTED_EDGE('',*,*,#7569,.F.);
#9509=ORIENTED_EDGE('',*,*,#7570,.F.);
#9510=ORIENTED_EDGE('',*,*,#7571,.T.);
#9511=ORIENTED_EDGE('',*,*,#7570,.T.);
#9512=ORIENTED_EDGE('',*,*,#7572,.F.);
#9513=ORIENTED_EDGE('',*,*,#7562,.F.);
#9514=ORIENTED_EDGE('',*,*,#7572,.T.);
#9515=ORIENTED_EDGE('',*,*,#7569,.T.);
#9516=ORIENTED_EDGE('',*,*,#7566,.T.);
#9517=ORIENTED_EDGE('',*,*,#7563,.T.);
#9518=ORIENTED_EDGE('',*,*,#7571,.F.);
#9519=ORIENTED_EDGE('',*,*,#7561,.F.);
#9520=ORIENTED_EDGE('',*,*,#7565,.F.);
#9521=ORIENTED_EDGE('',*,*,#7568,.F.);
#9522=ORIENTED_EDGE('',*,*,#7573,.F.);
#9523=ORIENTED_EDGE('',*,*,#7574,.T.);
#9524=ORIENTED_EDGE('',*,*,#7575,.F.);
#9525=ORIENTED_EDGE('',*,*,#7574,.F.);
#9526=ORIENTED_EDGE('',*,*,#7573,.T.);
#9527=ORIENTED_EDGE('',*,*,#7576,.F.);
#9528=ORIENTED_EDGE('',*,*,#7577,.F.);
#9529=ORIENTED_EDGE('',*,*,#7578,.T.);
#9530=ORIENTED_EDGE('',*,*,#7579,.F.);
#9531=ORIENTED_EDGE('',*,*,#7578,.F.);
#9532=ORIENTED_EDGE('',*,*,#7577,.T.);
#9533=ORIENTED_EDGE('',*,*,#7580,.F.);
#9534=ORIENTED_EDGE('',*,*,#7581,.F.);
#9535=ORIENTED_EDGE('',*,*,#7582,.T.);
#9536=ORIENTED_EDGE('',*,*,#7576,.T.);
#9537=ORIENTED_EDGE('',*,*,#7582,.F.);
#9538=ORIENTED_EDGE('',*,*,#7583,.F.);
#9539=ORIENTED_EDGE('',*,*,#7584,.T.);
#9540=ORIENTED_EDGE('',*,*,#7580,.T.);
#9541=ORIENTED_EDGE('',*,*,#7584,.F.);
#9542=ORIENTED_EDGE('',*,*,#7585,.T.);
#9543=ORIENTED_EDGE('',*,*,#7586,.T.);
#9544=ORIENTED_EDGE('',*,*,#7587,.F.);
#9545=ORIENTED_EDGE('',*,*,#7588,.F.);
#9546=ORIENTED_EDGE('',*,*,#7589,.T.);
#9547=ORIENTED_EDGE('',*,*,#7588,.T.);
#9548=ORIENTED_EDGE('',*,*,#7590,.F.);
#9549=ORIENTED_EDGE('',*,*,#7591,.F.);
#9550=ORIENTED_EDGE('',*,*,#7592,.T.);
#9551=ORIENTED_EDGE('',*,*,#7591,.T.);
#9552=ORIENTED_EDGE('',*,*,#7593,.F.);
#9553=ORIENTED_EDGE('',*,*,#7594,.F.);
#9554=ORIENTED_EDGE('',*,*,#7595,.T.);
#9555=ORIENTED_EDGE('',*,*,#7594,.T.);
#9556=ORIENTED_EDGE('',*,*,#7596,.F.);
#9557=ORIENTED_EDGE('',*,*,#7586,.F.);
#9558=ORIENTED_EDGE('',*,*,#7596,.T.);
#9559=ORIENTED_EDGE('',*,*,#7593,.T.);
#9560=ORIENTED_EDGE('',*,*,#7590,.T.);
#9561=ORIENTED_EDGE('',*,*,#7587,.T.);
#9562=ORIENTED_EDGE('',*,*,#7575,.T.);
#9563=ORIENTED_EDGE('',*,*,#7579,.T.);
#9564=ORIENTED_EDGE('',*,*,#7595,.F.);
#9565=ORIENTED_EDGE('',*,*,#7585,.F.);
#9566=ORIENTED_EDGE('',*,*,#7589,.F.);
#9567=ORIENTED_EDGE('',*,*,#7592,.F.);
#9568=ORIENTED_EDGE('',*,*,#7581,.T.);
#9569=ORIENTED_EDGE('',*,*,#7583,.T.);
#9570=ORIENTED_EDGE('',*,*,#7597,.T.);
#9571=ORIENTED_EDGE('',*,*,#7598,.T.);
#9572=ORIENTED_EDGE('',*,*,#7599,.F.);
#9573=ORIENTED_EDGE('',*,*,#7600,.F.);
#9574=ORIENTED_EDGE('',*,*,#7601,.T.);
#9575=ORIENTED_EDGE('',*,*,#7600,.T.);
#9576=ORIENTED_EDGE('',*,*,#7602,.F.);
#9577=ORIENTED_EDGE('',*,*,#7603,.F.);
#9578=ORIENTED_EDGE('',*,*,#7604,.T.);
#9579=ORIENTED_EDGE('',*,*,#7603,.T.);
#9580=ORIENTED_EDGE('',*,*,#7605,.F.);
#9581=ORIENTED_EDGE('',*,*,#7606,.F.);
#9582=ORIENTED_EDGE('',*,*,#7607,.T.);
#9583=ORIENTED_EDGE('',*,*,#7606,.T.);
#9584=ORIENTED_EDGE('',*,*,#7608,.F.);
#9585=ORIENTED_EDGE('',*,*,#7598,.F.);
#9586=ORIENTED_EDGE('',*,*,#7608,.T.);
#9587=ORIENTED_EDGE('',*,*,#7605,.T.);
#9588=ORIENTED_EDGE('',*,*,#7602,.T.);
#9589=ORIENTED_EDGE('',*,*,#7599,.T.);
#9590=ORIENTED_EDGE('',*,*,#7607,.F.);
#9591=ORIENTED_EDGE('',*,*,#7597,.F.);
#9592=ORIENTED_EDGE('',*,*,#7601,.F.);
#9593=ORIENTED_EDGE('',*,*,#7604,.F.);
#9594=ORIENTED_EDGE('',*,*,#7609,.F.);
#9595=ORIENTED_EDGE('',*,*,#7610,.T.);
#9596=ORIENTED_EDGE('',*,*,#7611,.F.);
#9597=ORIENTED_EDGE('',*,*,#7610,.F.);
#9598=ORIENTED_EDGE('',*,*,#7612,.F.);
#9599=ORIENTED_EDGE('',*,*,#7613,.T.);
#9600=ORIENTED_EDGE('',*,*,#7614,.F.);
#9601=ORIENTED_EDGE('',*,*,#7613,.F.);
#9602=ORIENTED_EDGE('',*,*,#7615,.F.);
#9603=ORIENTED_EDGE('',*,*,#7616,.T.);
#9604=ORIENTED_EDGE('',*,*,#7617,.F.);
#9605=ORIENTED_EDGE('',*,*,#7616,.F.);
#9606=ORIENTED_EDGE('',*,*,#7618,.F.);
#9607=ORIENTED_EDGE('',*,*,#7619,.T.);
#9608=ORIENTED_EDGE('',*,*,#7620,.F.);
#9609=ORIENTED_EDGE('',*,*,#7619,.F.);
#9610=ORIENTED_EDGE('',*,*,#7621,.F.);
#9611=ORIENTED_EDGE('',*,*,#7622,.T.);
#9612=ORIENTED_EDGE('',*,*,#7623,.F.);
#9613=ORIENTED_EDGE('',*,*,#7622,.F.);
#9614=ORIENTED_EDGE('',*,*,#7624,.F.);
#9615=ORIENTED_EDGE('',*,*,#7625,.T.);
#9616=ORIENTED_EDGE('',*,*,#7626,.F.);
#9617=ORIENTED_EDGE('',*,*,#7625,.F.);
#9618=ORIENTED_EDGE('',*,*,#7627,.F.);
#9619=ORIENTED_EDGE('',*,*,#7628,.T.);
#9620=ORIENTED_EDGE('',*,*,#7629,.F.);
#9621=ORIENTED_EDGE('',*,*,#7628,.F.);
#9622=ORIENTED_EDGE('',*,*,#7630,.F.);
#9623=ORIENTED_EDGE('',*,*,#7631,.F.);
#9624=ORIENTED_EDGE('',*,*,#7632,.T.);
#9625=ORIENTED_EDGE('',*,*,#7633,.F.);
#9626=ORIENTED_EDGE('',*,*,#7614,.T.);
#9627=ORIENTED_EDGE('',*,*,#7634,.F.);
#9628=ORIENTED_EDGE('',*,*,#7635,.F.);
#9629=ORIENTED_EDGE('',*,*,#7636,.F.);
#9630=ORIENTED_EDGE('',*,*,#7637,.F.);
#9631=ORIENTED_EDGE('',*,*,#7611,.T.);
#9632=ORIENTED_EDGE('',*,*,#7638,.F.);
#9633=ORIENTED_EDGE('',*,*,#7636,.T.);
#9634=ORIENTED_EDGE('',*,*,#7639,.F.);
#9635=ORIENTED_EDGE('',*,*,#7640,.F.);
#9636=ORIENTED_EDGE('',*,*,#7641,.F.);
#9637=ORIENTED_EDGE('',*,*,#7642,.T.);
#9638=ORIENTED_EDGE('',*,*,#7643,.F.);
#9639=ORIENTED_EDGE('',*,*,#7632,.F.);
#9640=ORIENTED_EDGE('',*,*,#7644,.T.);
#9641=ORIENTED_EDGE('',*,*,#7645,.F.);
#9642=ORIENTED_EDGE('',*,*,#7646,.F.);
#9643=ORIENTED_EDGE('',*,*,#7637,.T.);
#9644=ORIENTED_EDGE('',*,*,#7638,.T.);
#9645=ORIENTED_EDGE('',*,*,#7647,.T.);
#9646=ORIENTED_EDGE('',*,*,#7641,.T.);
#9647=ORIENTED_EDGE('',*,*,#7631,.T.);
#9648=ORIENTED_EDGE('',*,*,#7627,.T.);
#9649=ORIENTED_EDGE('',*,*,#7624,.T.);
#9650=ORIENTED_EDGE('',*,*,#7621,.T.);
#9651=ORIENTED_EDGE('',*,*,#7618,.T.);
#9652=ORIENTED_EDGE('',*,*,#7615,.T.);
#9653=ORIENTED_EDGE('',*,*,#7630,.T.);
#9654=ORIENTED_EDGE('',*,*,#7648,.T.);
#9655=ORIENTED_EDGE('',*,*,#7649,.F.);
#9656=ORIENTED_EDGE('',*,*,#7644,.F.);
#9657=ORIENTED_EDGE('',*,*,#7650,.T.);
#9658=ORIENTED_EDGE('',*,*,#7651,.F.);
#9659=ORIENTED_EDGE('',*,*,#7648,.F.);
#9660=ORIENTED_EDGE('',*,*,#7633,.T.);
#9661=ORIENTED_EDGE('',*,*,#7643,.T.);
#9662=ORIENTED_EDGE('',*,*,#7652,.T.);
#9663=ORIENTED_EDGE('',*,*,#7639,.T.);
#9664=ORIENTED_EDGE('',*,*,#7635,.T.);
#9665=ORIENTED_EDGE('',*,*,#7629,.T.);
#9666=ORIENTED_EDGE('',*,*,#7626,.T.);
#9667=ORIENTED_EDGE('',*,*,#7623,.T.);
#9668=ORIENTED_EDGE('',*,*,#7620,.T.);
#9669=ORIENTED_EDGE('',*,*,#7617,.T.);
#9670=ORIENTED_EDGE('',*,*,#7634,.T.);
#9671=ORIENTED_EDGE('',*,*,#7646,.T.);
#9672=ORIENTED_EDGE('',*,*,#7653,.F.);
#9673=ORIENTED_EDGE('',*,*,#7650,.F.);
#9674=ORIENTED_EDGE('',*,*,#7653,.T.);
#9675=ORIENTED_EDGE('',*,*,#7645,.T.);
#9676=ORIENTED_EDGE('',*,*,#7649,.T.);
#9677=ORIENTED_EDGE('',*,*,#7651,.T.);
#9678=ORIENTED_EDGE('',*,*,#7652,.F.);
#9679=ORIENTED_EDGE('',*,*,#7642,.F.);
#9680=ORIENTED_EDGE('',*,*,#7647,.F.);
#9681=ORIENTED_EDGE('',*,*,#7640,.T.);
#9682=ORIENTED_EDGE('',*,*,#7609,.T.);
#9683=ORIENTED_EDGE('',*,*,#7612,.T.);
#9684=ORIENTED_EDGE('',*,*,#7654,.F.);
#9685=ORIENTED_EDGE('',*,*,#7655,.T.);
#9686=ORIENTED_EDGE('',*,*,#7656,.F.);
#9687=ORIENTED_EDGE('',*,*,#7655,.F.);
#9688=ORIENTED_EDGE('',*,*,#7657,.F.);
#9689=ORIENTED_EDGE('',*,*,#7658,.T.);
#9690=ORIENTED_EDGE('',*,*,#7659,.F.);
#9691=ORIENTED_EDGE('',*,*,#7658,.F.);
#9692=ORIENTED_EDGE('',*,*,#7660,.F.);
#9693=ORIENTED_EDGE('',*,*,#7661,.T.);
#9694=ORIENTED_EDGE('',*,*,#7662,.F.);
#9695=ORIENTED_EDGE('',*,*,#7661,.F.);
#9696=ORIENTED_EDGE('',*,*,#7663,.F.);
#9697=ORIENTED_EDGE('',*,*,#7664,.T.);
#9698=ORIENTED_EDGE('',*,*,#7665,.F.);
#9699=ORIENTED_EDGE('',*,*,#7664,.F.);
#9700=ORIENTED_EDGE('',*,*,#7666,.F.);
#9701=ORIENTED_EDGE('',*,*,#7667,.T.);
#9702=ORIENTED_EDGE('',*,*,#7668,.F.);
#9703=ORIENTED_EDGE('',*,*,#7667,.F.);
#9704=ORIENTED_EDGE('',*,*,#7666,.T.);
#9705=ORIENTED_EDGE('',*,*,#7669,.T.);
#9706=ORIENTED_EDGE('',*,*,#7669,.F.);
#9707=ORIENTED_EDGE('',*,*,#7670,.T.);
#9708=ORIENTED_EDGE('',*,*,#7671,.T.);
#9709=ORIENTED_EDGE('',*,*,#7670,.F.);
#9710=ORIENTED_EDGE('',*,*,#7672,.F.);
#9711=ORIENTED_EDGE('',*,*,#7673,.T.);
#9712=ORIENTED_EDGE('',*,*,#7674,.T.);
#9713=ORIENTED_EDGE('',*,*,#7673,.F.);
#9714=ORIENTED_EDGE('',*,*,#7672,.T.);
#9715=ORIENTED_EDGE('',*,*,#7668,.T.);
#9716=ORIENTED_EDGE('',*,*,#7665,.T.);
#9717=ORIENTED_EDGE('',*,*,#7662,.T.);
#9718=ORIENTED_EDGE('',*,*,#7659,.T.);
#9719=ORIENTED_EDGE('',*,*,#7656,.T.);
#9720=ORIENTED_EDGE('',*,*,#7674,.F.);
#9721=ORIENTED_EDGE('',*,*,#7671,.F.);
#9722=ORIENTED_EDGE('',*,*,#7663,.T.);
#9723=ORIENTED_EDGE('',*,*,#7660,.T.);
#9724=ORIENTED_EDGE('',*,*,#7657,.T.);
#9725=ORIENTED_EDGE('',*,*,#7654,.T.);
#9726=ORIENTED_EDGE('',*,*,#7675,.F.);
#9727=ORIENTED_EDGE('',*,*,#7676,.T.);
#9728=ORIENTED_EDGE('',*,*,#7677,.F.);
#9729=ORIENTED_EDGE('',*,*,#7676,.F.);
#9730=ORIENTED_EDGE('',*,*,#7678,.F.);
#9731=ORIENTED_EDGE('',*,*,#7679,.T.);
#9732=ORIENTED_EDGE('',*,*,#7680,.F.);
#9733=ORIENTED_EDGE('',*,*,#7679,.F.);
#9734=ORIENTED_EDGE('',*,*,#7681,.F.);
#9735=ORIENTED_EDGE('',*,*,#7682,.T.);
#9736=ORIENTED_EDGE('',*,*,#7683,.F.);
#9737=ORIENTED_EDGE('',*,*,#7682,.F.);
#9738=ORIENTED_EDGE('',*,*,#7684,.F.);
#9739=ORIENTED_EDGE('',*,*,#7685,.T.);
#9740=ORIENTED_EDGE('',*,*,#7686,.F.);
#9741=ORIENTED_EDGE('',*,*,#7685,.F.);
#9742=ORIENTED_EDGE('',*,*,#7687,.F.);
#9743=ORIENTED_EDGE('',*,*,#7688,.T.);
#9744=ORIENTED_EDGE('',*,*,#7689,.T.);
#9745=ORIENTED_EDGE('',*,*,#7688,.F.);
#9746=ORIENTED_EDGE('',*,*,#7689,.F.);
#9747=ORIENTED_EDGE('',*,*,#7690,.F.);
#9748=ORIENTED_EDGE('',*,*,#7691,.F.);
#9749=ORIENTED_EDGE('',*,*,#7692,.T.);
#9750=ORIENTED_EDGE('',*,*,#7690,.T.);
#9751=ORIENTED_EDGE('',*,*,#7692,.F.);
#9752=ORIENTED_EDGE('',*,*,#7693,.F.);
#9753=ORIENTED_EDGE('',*,*,#7694,.T.);
#9754=ORIENTED_EDGE('',*,*,#7695,.T.);
#9755=ORIENTED_EDGE('',*,*,#7694,.F.);
#9756=ORIENTED_EDGE('',*,*,#7693,.T.);
#9757=ORIENTED_EDGE('',*,*,#7691,.T.);
#9758=ORIENTED_EDGE('',*,*,#7686,.T.);
#9759=ORIENTED_EDGE('',*,*,#7683,.T.);
#9760=ORIENTED_EDGE('',*,*,#7680,.T.);
#9761=ORIENTED_EDGE('',*,*,#7677,.T.);
#9762=ORIENTED_EDGE('',*,*,#7695,.F.);
#9763=ORIENTED_EDGE('',*,*,#7687,.T.);
#9764=ORIENTED_EDGE('',*,*,#7684,.T.);
#9765=ORIENTED_EDGE('',*,*,#7681,.T.);
#9766=ORIENTED_EDGE('',*,*,#7678,.T.);
#9767=ORIENTED_EDGE('',*,*,#7675,.T.);
#9768=ORIENTED_EDGE('',*,*,#7696,.F.);
#9769=ORIENTED_EDGE('',*,*,#7697,.T.);
#9770=ORIENTED_EDGE('',*,*,#7698,.F.);
#9771=ORIENTED_EDGE('',*,*,#7697,.F.);
#9772=ORIENTED_EDGE('',*,*,#7699,.F.);
#9773=ORIENTED_EDGE('',*,*,#7700,.T.);
#9774=ORIENTED_EDGE('',*,*,#7701,.F.);
#9775=ORIENTED_EDGE('',*,*,#7700,.F.);
#9776=ORIENTED_EDGE('',*,*,#7702,.F.);
#9777=ORIENTED_EDGE('',*,*,#7703,.T.);
#9778=ORIENTED_EDGE('',*,*,#7704,.F.);
#9779=ORIENTED_EDGE('',*,*,#7703,.F.);
#9780=ORIENTED_EDGE('',*,*,#7705,.F.);
#9781=ORIENTED_EDGE('',*,*,#7706,.T.);
#9782=ORIENTED_EDGE('',*,*,#7707,.F.);
#9783=ORIENTED_EDGE('',*,*,#7706,.F.);
#9784=ORIENTED_EDGE('',*,*,#7708,.F.);
#9785=ORIENTED_EDGE('',*,*,#7709,.T.);
#9786=ORIENTED_EDGE('',*,*,#7710,.F.);
#9787=ORIENTED_EDGE('',*,*,#7709,.F.);
#9788=ORIENTED_EDGE('',*,*,#7711,.F.);
#9789=ORIENTED_EDGE('',*,*,#7712,.T.);
#9790=ORIENTED_EDGE('',*,*,#7713,.F.);
#9791=ORIENTED_EDGE('',*,*,#7712,.F.);
#9792=ORIENTED_EDGE('',*,*,#7714,.F.);
#9793=ORIENTED_EDGE('',*,*,#7715,.T.);
#9794=ORIENTED_EDGE('',*,*,#7716,.F.);
#9795=ORIENTED_EDGE('',*,*,#7715,.F.);
#9796=ORIENTED_EDGE('',*,*,#7717,.F.);
#9797=ORIENTED_EDGE('',*,*,#7718,.F.);
#9798=ORIENTED_EDGE('',*,*,#7719,.T.);
#9799=ORIENTED_EDGE('',*,*,#7720,.F.);
#9800=ORIENTED_EDGE('',*,*,#7701,.T.);
#9801=ORIENTED_EDGE('',*,*,#7721,.F.);
#9802=ORIENTED_EDGE('',*,*,#7722,.F.);
#9803=ORIENTED_EDGE('',*,*,#7723,.F.);
#9804=ORIENTED_EDGE('',*,*,#7724,.F.);
#9805=ORIENTED_EDGE('',*,*,#7698,.T.);
#9806=ORIENTED_EDGE('',*,*,#7725,.F.);
#9807=ORIENTED_EDGE('',*,*,#7723,.T.);
#9808=ORIENTED_EDGE('',*,*,#7726,.F.);
#9809=ORIENTED_EDGE('',*,*,#7727,.F.);
#9810=ORIENTED_EDGE('',*,*,#7728,.F.);
#9811=ORIENTED_EDGE('',*,*,#7729,.T.);
#9812=ORIENTED_EDGE('',*,*,#7730,.F.);
#9813=ORIENTED_EDGE('',*,*,#7719,.F.);
#9814=ORIENTED_EDGE('',*,*,#7731,.T.);
#9815=ORIENTED_EDGE('',*,*,#7732,.F.);
#9816=ORIENTED_EDGE('',*,*,#7733,.F.);
#9817=ORIENTED_EDGE('',*,*,#7724,.T.);
#9818=ORIENTED_EDGE('',*,*,#7725,.T.);
#9819=ORIENTED_EDGE('',*,*,#7734,.T.);
#9820=ORIENTED_EDGE('',*,*,#7728,.T.);
#9821=ORIENTED_EDGE('',*,*,#7718,.T.);
#9822=ORIENTED_EDGE('',*,*,#7714,.T.);
#9823=ORIENTED_EDGE('',*,*,#7711,.T.);
#9824=ORIENTED_EDGE('',*,*,#7708,.T.);
#9825=ORIENTED_EDGE('',*,*,#7705,.T.);
#9826=ORIENTED_EDGE('',*,*,#7702,.T.);
#9827=ORIENTED_EDGE('',*,*,#7717,.T.);
#9828=ORIENTED_EDGE('',*,*,#7735,.T.);
#9829=ORIENTED_EDGE('',*,*,#7736,.F.);
#9830=ORIENTED_EDGE('',*,*,#7731,.F.);
#9831=ORIENTED_EDGE('',*,*,#7737,.T.);
#9832=ORIENTED_EDGE('',*,*,#7738,.F.);
#9833=ORIENTED_EDGE('',*,*,#7735,.F.);
#9834=ORIENTED_EDGE('',*,*,#7720,.T.);
#9835=ORIENTED_EDGE('',*,*,#7730,.T.);
#9836=ORIENTED_EDGE('',*,*,#7739,.T.);
#9837=ORIENTED_EDGE('',*,*,#7726,.T.);
#9838=ORIENTED_EDGE('',*,*,#7722,.T.);
#9839=ORIENTED_EDGE('',*,*,#7716,.T.);
#9840=ORIENTED_EDGE('',*,*,#7713,.T.);
#9841=ORIENTED_EDGE('',*,*,#7710,.T.);
#9842=ORIENTED_EDGE('',*,*,#7707,.T.);
#9843=ORIENTED_EDGE('',*,*,#7704,.T.);
#9844=ORIENTED_EDGE('',*,*,#7721,.T.);
#9845=ORIENTED_EDGE('',*,*,#7733,.T.);
#9846=ORIENTED_EDGE('',*,*,#7740,.F.);
#9847=ORIENTED_EDGE('',*,*,#7737,.F.);
#9848=ORIENTED_EDGE('',*,*,#7740,.T.);
#9849=ORIENTED_EDGE('',*,*,#7732,.T.);
#9850=ORIENTED_EDGE('',*,*,#7736,.T.);
#9851=ORIENTED_EDGE('',*,*,#7738,.T.);
#9852=ORIENTED_EDGE('',*,*,#7739,.F.);
#9853=ORIENTED_EDGE('',*,*,#7729,.F.);
#9854=ORIENTED_EDGE('',*,*,#7734,.F.);
#9855=ORIENTED_EDGE('',*,*,#7727,.T.);
#9856=ORIENTED_EDGE('',*,*,#7696,.T.);
#9857=ORIENTED_EDGE('',*,*,#7699,.T.);
#9858=ORIENTED_EDGE('',*,*,#7741,.F.);
#9859=ORIENTED_EDGE('',*,*,#7742,.T.);
#9860=ORIENTED_EDGE('',*,*,#7743,.F.);
#9861=ORIENTED_EDGE('',*,*,#7742,.F.);
#9862=ORIENTED_EDGE('',*,*,#7744,.F.);
#9863=ORIENTED_EDGE('',*,*,#7745,.T.);
#9864=ORIENTED_EDGE('',*,*,#7746,.F.);
#9865=ORIENTED_EDGE('',*,*,#7745,.F.);
#9866=ORIENTED_EDGE('',*,*,#7747,.F.);
#9867=ORIENTED_EDGE('',*,*,#7748,.T.);
#9868=ORIENTED_EDGE('',*,*,#7749,.F.);
#9869=ORIENTED_EDGE('',*,*,#7748,.F.);
#9870=ORIENTED_EDGE('',*,*,#7750,.F.);
#9871=ORIENTED_EDGE('',*,*,#7751,.T.);
#9872=ORIENTED_EDGE('',*,*,#7752,.F.);
#9873=ORIENTED_EDGE('',*,*,#7751,.F.);
#9874=ORIENTED_EDGE('',*,*,#7753,.F.);
#9875=ORIENTED_EDGE('',*,*,#7754,.T.);
#9876=ORIENTED_EDGE('',*,*,#7755,.F.);
#9877=ORIENTED_EDGE('',*,*,#7754,.F.);
#9878=ORIENTED_EDGE('',*,*,#7753,.T.);
#9879=ORIENTED_EDGE('',*,*,#7756,.T.);
#9880=ORIENTED_EDGE('',*,*,#7756,.F.);
#9881=ORIENTED_EDGE('',*,*,#7757,.T.);
#9882=ORIENTED_EDGE('',*,*,#7758,.T.);
#9883=ORIENTED_EDGE('',*,*,#7757,.F.);
#9884=ORIENTED_EDGE('',*,*,#7759,.F.);
#9885=ORIENTED_EDGE('',*,*,#7760,.T.);
#9886=ORIENTED_EDGE('',*,*,#7761,.T.);
#9887=ORIENTED_EDGE('',*,*,#7760,.F.);
#9888=ORIENTED_EDGE('',*,*,#7759,.T.);
#9889=ORIENTED_EDGE('',*,*,#7755,.T.);
#9890=ORIENTED_EDGE('',*,*,#7752,.T.);
#9891=ORIENTED_EDGE('',*,*,#7749,.T.);
#9892=ORIENTED_EDGE('',*,*,#7746,.T.);
#9893=ORIENTED_EDGE('',*,*,#7743,.T.);
#9894=ORIENTED_EDGE('',*,*,#7761,.F.);
#9895=ORIENTED_EDGE('',*,*,#7758,.F.);
#9896=ORIENTED_EDGE('',*,*,#7750,.T.);
#9897=ORIENTED_EDGE('',*,*,#7747,.T.);
#9898=ORIENTED_EDGE('',*,*,#7744,.T.);
#9899=ORIENTED_EDGE('',*,*,#7741,.T.);
#9900=ORIENTED_EDGE('',*,*,#7762,.F.);
#9901=ORIENTED_EDGE('',*,*,#7763,.T.);
#9902=ORIENTED_EDGE('',*,*,#7764,.F.);
#9903=ORIENTED_EDGE('',*,*,#7763,.F.);
#9904=ORIENTED_EDGE('',*,*,#7765,.F.);
#9905=ORIENTED_EDGE('',*,*,#7766,.T.);
#9906=ORIENTED_EDGE('',*,*,#7767,.F.);
#9907=ORIENTED_EDGE('',*,*,#7766,.F.);
#9908=ORIENTED_EDGE('',*,*,#7768,.F.);
#9909=ORIENTED_EDGE('',*,*,#7769,.T.);
#9910=ORIENTED_EDGE('',*,*,#7770,.F.);
#9911=ORIENTED_EDGE('',*,*,#7769,.F.);
#9912=ORIENTED_EDGE('',*,*,#7771,.F.);
#9913=ORIENTED_EDGE('',*,*,#7772,.T.);
#9914=ORIENTED_EDGE('',*,*,#7773,.F.);
#9915=ORIENTED_EDGE('',*,*,#7772,.F.);
#9916=ORIENTED_EDGE('',*,*,#7774,.F.);
#9917=ORIENTED_EDGE('',*,*,#7775,.T.);
#9918=ORIENTED_EDGE('',*,*,#7776,.T.);
#9919=ORIENTED_EDGE('',*,*,#7775,.F.);
#9920=ORIENTED_EDGE('',*,*,#7776,.F.);
#9921=ORIENTED_EDGE('',*,*,#7777,.F.);
#9922=ORIENTED_EDGE('',*,*,#7778,.F.);
#9923=ORIENTED_EDGE('',*,*,#7779,.T.);
#9924=ORIENTED_EDGE('',*,*,#7777,.T.);
#9925=ORIENTED_EDGE('',*,*,#7779,.F.);
#9926=ORIENTED_EDGE('',*,*,#7780,.F.);
#9927=ORIENTED_EDGE('',*,*,#7781,.T.);
#9928=ORIENTED_EDGE('',*,*,#7782,.T.);
#9929=ORIENTED_EDGE('',*,*,#7781,.F.);
#9930=ORIENTED_EDGE('',*,*,#7780,.T.);
#9931=ORIENTED_EDGE('',*,*,#7778,.T.);
#9932=ORIENTED_EDGE('',*,*,#7773,.T.);
#9933=ORIENTED_EDGE('',*,*,#7770,.T.);
#9934=ORIENTED_EDGE('',*,*,#7767,.T.);
#9935=ORIENTED_EDGE('',*,*,#7764,.T.);
#9936=ORIENTED_EDGE('',*,*,#7782,.F.);
#9937=ORIENTED_EDGE('',*,*,#7774,.T.);
#9938=ORIENTED_EDGE('',*,*,#7771,.T.);
#9939=ORIENTED_EDGE('',*,*,#7768,.T.);
#9940=ORIENTED_EDGE('',*,*,#7765,.T.);
#9941=ORIENTED_EDGE('',*,*,#7762,.T.);
#9942=ORIENTED_EDGE('',*,*,#7783,.F.);
#9943=ORIENTED_EDGE('',*,*,#7784,.T.);
#9944=ORIENTED_EDGE('',*,*,#7785,.F.);
#9945=ORIENTED_EDGE('',*,*,#7786,.F.);
#9946=ORIENTED_EDGE('',*,*,#7787,.F.);
#9947=ORIENTED_EDGE('',*,*,#7788,.T.);
#9948=ORIENTED_EDGE('',*,*,#7789,.F.);
#9949=ORIENTED_EDGE('',*,*,#7784,.F.);
#9950=ORIENTED_EDGE('',*,*,#7790,.F.);
#9951=ORIENTED_EDGE('',*,*,#7791,.T.);
#9952=ORIENTED_EDGE('',*,*,#7792,.F.);
#9953=ORIENTED_EDGE('',*,*,#7788,.F.);
#9954=ORIENTED_EDGE('',*,*,#7793,.F.);
#9955=ORIENTED_EDGE('',*,*,#7794,.T.);
#9956=ORIENTED_EDGE('',*,*,#7795,.F.);
#9957=ORIENTED_EDGE('',*,*,#7791,.F.);
#9958=ORIENTED_EDGE('',*,*,#7796,.F.);
#9959=ORIENTED_EDGE('',*,*,#7797,.T.);
#9960=ORIENTED_EDGE('',*,*,#7798,.F.);
#9961=ORIENTED_EDGE('',*,*,#7794,.F.);
#9962=ORIENTED_EDGE('',*,*,#7799,.F.);
#9963=ORIENTED_EDGE('',*,*,#7800,.T.);
#9964=ORIENTED_EDGE('',*,*,#7801,.F.);
#9965=ORIENTED_EDGE('',*,*,#7797,.F.);
#9966=ORIENTED_EDGE('',*,*,#7802,.F.);
#9967=ORIENTED_EDGE('',*,*,#7803,.T.);
#9968=ORIENTED_EDGE('',*,*,#7804,.F.);
#9969=ORIENTED_EDGE('',*,*,#7800,.F.);
#9970=ORIENTED_EDGE('',*,*,#7805,.F.);
#9971=ORIENTED_EDGE('',*,*,#7806,.T.);
#9972=ORIENTED_EDGE('',*,*,#7807,.F.);
#9973=ORIENTED_EDGE('',*,*,#7803,.F.);
#9974=ORIENTED_EDGE('',*,*,#7808,.F.);
#9975=ORIENTED_EDGE('',*,*,#7809,.F.);
#9976=ORIENTED_EDGE('',*,*,#7810,.F.);
#9977=ORIENTED_EDGE('',*,*,#7806,.F.);
#9978=ORIENTED_EDGE('',*,*,#7811,.F.);
#9979=ORIENTED_EDGE('',*,*,#7812,.T.);
#9980=ORIENTED_EDGE('',*,*,#7813,.F.);
#9981=ORIENTED_EDGE('',*,*,#7814,.F.);
#9982=ORIENTED_EDGE('',*,*,#7815,.F.);
#9983=ORIENTED_EDGE('',*,*,#7816,.T.);
#9984=ORIENTED_EDGE('',*,*,#7817,.F.);
#9985=ORIENTED_EDGE('',*,*,#7812,.F.);
#9986=ORIENTED_EDGE('',*,*,#7818,.F.);
#9987=ORIENTED_EDGE('',*,*,#7819,.T.);
#9988=ORIENTED_EDGE('',*,*,#7820,.F.);
#9989=ORIENTED_EDGE('',*,*,#7816,.F.);
#9990=ORIENTED_EDGE('',*,*,#7821,.F.);
#9991=ORIENTED_EDGE('',*,*,#7822,.T.);
#9992=ORIENTED_EDGE('',*,*,#7823,.F.);
#9993=ORIENTED_EDGE('',*,*,#7819,.F.);
#9994=ORIENTED_EDGE('',*,*,#7824,.F.);
#9995=ORIENTED_EDGE('',*,*,#7825,.T.);
#9996=ORIENTED_EDGE('',*,*,#7826,.F.);
#9997=ORIENTED_EDGE('',*,*,#7822,.F.);
#9998=ORIENTED_EDGE('',*,*,#7827,.F.);
#9999=ORIENTED_EDGE('',*,*,#7828,.T.);
#10000=ORIENTED_EDGE('',*,*,#7829,.F.);
#10001=ORIENTED_EDGE('',*,*,#7825,.F.);
#10002=ORIENTED_EDGE('',*,*,#7830,.F.);
#10003=ORIENTED_EDGE('',*,*,#7831,.T.);
#10004=ORIENTED_EDGE('',*,*,#7832,.F.);
#10005=ORIENTED_EDGE('',*,*,#7828,.F.);
#10006=ORIENTED_EDGE('',*,*,#7833,.F.);
#10007=ORIENTED_EDGE('',*,*,#7834,.T.);
#10008=ORIENTED_EDGE('',*,*,#7835,.F.);
#10009=ORIENTED_EDGE('',*,*,#7831,.F.);
#10010=ORIENTED_EDGE('',*,*,#7836,.F.);
#10011=ORIENTED_EDGE('',*,*,#7837,.F.);
#10012=ORIENTED_EDGE('',*,*,#7838,.F.);
#10013=ORIENTED_EDGE('',*,*,#7834,.F.);
#10014=ORIENTED_EDGE('',*,*,#7839,.F.);
#10015=ORIENTED_EDGE('',*,*,#7840,.T.);
#10016=ORIENTED_EDGE('',*,*,#7841,.F.);
#10017=ORIENTED_EDGE('',*,*,#7842,.F.);
#10018=ORIENTED_EDGE('',*,*,#7843,.F.);
#10019=ORIENTED_EDGE('',*,*,#7844,.T.);
#10020=ORIENTED_EDGE('',*,*,#7845,.F.);
#10021=ORIENTED_EDGE('',*,*,#7840,.F.);
#10022=ORIENTED_EDGE('',*,*,#7846,.F.);
#10023=ORIENTED_EDGE('',*,*,#7847,.T.);
#10024=ORIENTED_EDGE('',*,*,#7848,.F.);
#10025=ORIENTED_EDGE('',*,*,#7844,.F.);
#10026=ORIENTED_EDGE('',*,*,#7849,.F.);
#10027=ORIENTED_EDGE('',*,*,#7850,.T.);
#10028=ORIENTED_EDGE('',*,*,#7851,.F.);
#10029=ORIENTED_EDGE('',*,*,#7847,.F.);
#10030=ORIENTED_EDGE('',*,*,#7852,.F.);
#10031=ORIENTED_EDGE('',*,*,#7853,.T.);
#10032=ORIENTED_EDGE('',*,*,#7854,.F.);
#10033=ORIENTED_EDGE('',*,*,#7850,.F.);
#10034=ORIENTED_EDGE('',*,*,#7855,.F.);
#10035=ORIENTED_EDGE('',*,*,#7856,.T.);
#10036=ORIENTED_EDGE('',*,*,#7857,.F.);
#10037=ORIENTED_EDGE('',*,*,#7853,.F.);
#10038=ORIENTED_EDGE('',*,*,#7858,.F.);
#10039=ORIENTED_EDGE('',*,*,#7859,.T.);
#10040=ORIENTED_EDGE('',*,*,#7860,.F.);
#10041=ORIENTED_EDGE('',*,*,#7856,.F.);
#10042=ORIENTED_EDGE('',*,*,#7861,.F.);
#10043=ORIENTED_EDGE('',*,*,#7862,.T.);
#10044=ORIENTED_EDGE('',*,*,#7863,.F.);
#10045=ORIENTED_EDGE('',*,*,#7859,.F.);
#10046=ORIENTED_EDGE('',*,*,#7864,.F.);
#10047=ORIENTED_EDGE('',*,*,#7865,.F.);
#10048=ORIENTED_EDGE('',*,*,#7866,.F.);
#10049=ORIENTED_EDGE('',*,*,#7862,.F.);
#10050=ORIENTED_EDGE('',*,*,#7867,.F.);
#10051=ORIENTED_EDGE('',*,*,#7868,.T.);
#10052=ORIENTED_EDGE('',*,*,#7869,.F.);
#10053=ORIENTED_EDGE('',*,*,#7870,.F.);
#10054=ORIENTED_EDGE('',*,*,#7871,.F.);
#10055=ORIENTED_EDGE('',*,*,#7872,.T.);
#10056=ORIENTED_EDGE('',*,*,#7873,.F.);
#10057=ORIENTED_EDGE('',*,*,#7868,.F.);
#10058=ORIENTED_EDGE('',*,*,#7874,.F.);
#10059=ORIENTED_EDGE('',*,*,#7875,.T.);
#10060=ORIENTED_EDGE('',*,*,#7876,.F.);
#10061=ORIENTED_EDGE('',*,*,#7872,.F.);
#10062=ORIENTED_EDGE('',*,*,#7877,.F.);
#10063=ORIENTED_EDGE('',*,*,#7878,.T.);
#10064=ORIENTED_EDGE('',*,*,#7879,.F.);
#10065=ORIENTED_EDGE('',*,*,#7875,.F.);
#10066=ORIENTED_EDGE('',*,*,#7880,.F.);
#10067=ORIENTED_EDGE('',*,*,#7881,.T.);
#10068=ORIENTED_EDGE('',*,*,#7882,.F.);
#10069=ORIENTED_EDGE('',*,*,#7878,.F.);
#10070=ORIENTED_EDGE('',*,*,#7883,.F.);
#10071=ORIENTED_EDGE('',*,*,#7884,.T.);
#10072=ORIENTED_EDGE('',*,*,#7885,.F.);
#10073=ORIENTED_EDGE('',*,*,#7881,.F.);
#10074=ORIENTED_EDGE('',*,*,#7886,.F.);
#10075=ORIENTED_EDGE('',*,*,#7887,.T.);
#10076=ORIENTED_EDGE('',*,*,#7888,.F.);
#10077=ORIENTED_EDGE('',*,*,#7884,.F.);
#10078=ORIENTED_EDGE('',*,*,#7889,.F.);
#10079=ORIENTED_EDGE('',*,*,#7890,.T.);
#10080=ORIENTED_EDGE('',*,*,#7891,.F.);
#10081=ORIENTED_EDGE('',*,*,#7887,.F.);
#10082=ORIENTED_EDGE('',*,*,#7892,.F.);
#10083=ORIENTED_EDGE('',*,*,#7893,.F.);
#10084=ORIENTED_EDGE('',*,*,#7894,.F.);
#10085=ORIENTED_EDGE('',*,*,#7890,.F.);
#10086=ORIENTED_EDGE('',*,*,#7895,.F.);
#10087=ORIENTED_EDGE('',*,*,#7896,.T.);
#10088=ORIENTED_EDGE('',*,*,#7897,.F.);
#10089=ORIENTED_EDGE('',*,*,#7896,.F.);
#10090=ORIENTED_EDGE('',*,*,#7809,.T.);
#10091=ORIENTED_EDGE('',*,*,#7898,.T.);
#10092=ORIENTED_EDGE('',*,*,#7899,.T.);
#10093=ORIENTED_EDGE('',*,*,#7900,.F.);
#10094=ORIENTED_EDGE('',*,*,#7786,.T.);
#10095=ORIENTED_EDGE('',*,*,#7901,.F.);
#10096=ORIENTED_EDGE('',*,*,#7902,.F.);
#10097=ORIENTED_EDGE('',*,*,#7903,.T.);
#10098=ORIENTED_EDGE('',*,*,#7837,.T.);
#10099=ORIENTED_EDGE('',*,*,#7904,.T.);
#10100=ORIENTED_EDGE('',*,*,#7902,.T.);
#10101=ORIENTED_EDGE('',*,*,#7905,.F.);
#10102=ORIENTED_EDGE('',*,*,#7814,.T.);
#10103=ORIENTED_EDGE('',*,*,#7906,.F.);
#10104=ORIENTED_EDGE('',*,*,#7907,.F.);
#10105=ORIENTED_EDGE('',*,*,#7908,.T.);
#10106=ORIENTED_EDGE('',*,*,#7865,.T.);
#10107=ORIENTED_EDGE('',*,*,#7909,.T.);
#10108=ORIENTED_EDGE('',*,*,#7907,.T.);
#10109=ORIENTED_EDGE('',*,*,#7910,.F.);
#10110=ORIENTED_EDGE('',*,*,#7842,.T.);
#10111=ORIENTED_EDGE('',*,*,#7911,.F.);
#10112=ORIENTED_EDGE('',*,*,#7912,.F.);
#10113=ORIENTED_EDGE('',*,*,#7913,.T.);
#10114=ORIENTED_EDGE('',*,*,#7893,.T.);
#10115=ORIENTED_EDGE('',*,*,#7914,.T.);
#10116=ORIENTED_EDGE('',*,*,#7912,.T.);
#10117=ORIENTED_EDGE('',*,*,#7915,.F.);
#10118=ORIENTED_EDGE('',*,*,#7870,.T.);
#10119=ORIENTED_EDGE('',*,*,#7916,.F.);
#10120=ORIENTED_EDGE('',*,*,#7899,.F.);
#10121=ORIENTED_EDGE('',*,*,#7917,.T.);
#10122=ORIENTED_EDGE('',*,*,#7785,.T.);
#10123=ORIENTED_EDGE('',*,*,#7789,.T.);
#10124=ORIENTED_EDGE('',*,*,#7792,.T.);
#10125=ORIENTED_EDGE('',*,*,#7795,.T.);
#10126=ORIENTED_EDGE('',*,*,#7798,.T.);
#10127=ORIENTED_EDGE('',*,*,#7801,.T.);
#10128=ORIENTED_EDGE('',*,*,#7804,.T.);
#10129=ORIENTED_EDGE('',*,*,#7807,.T.);
#10130=ORIENTED_EDGE('',*,*,#7810,.T.);
#10131=ORIENTED_EDGE('',*,*,#7900,.T.);
#10132=ORIENTED_EDGE('',*,*,#7916,.T.);
#10133=ORIENTED_EDGE('',*,*,#7869,.T.);
#10134=ORIENTED_EDGE('',*,*,#7873,.T.);
#10135=ORIENTED_EDGE('',*,*,#7876,.T.);
#10136=ORIENTED_EDGE('',*,*,#7879,.T.);
#10137=ORIENTED_EDGE('',*,*,#7882,.T.);
#10138=ORIENTED_EDGE('',*,*,#7885,.T.);
#10139=ORIENTED_EDGE('',*,*,#7888,.T.);
#10140=ORIENTED_EDGE('',*,*,#7891,.T.);
#10141=ORIENTED_EDGE('',*,*,#7894,.T.);
#10142=ORIENTED_EDGE('',*,*,#7915,.T.);
#10143=ORIENTED_EDGE('',*,*,#7911,.T.);
#10144=ORIENTED_EDGE('',*,*,#7841,.T.);
#10145=ORIENTED_EDGE('',*,*,#7845,.T.);
#10146=ORIENTED_EDGE('',*,*,#7848,.T.);
#10147=ORIENTED_EDGE('',*,*,#7851,.T.);
#10148=ORIENTED_EDGE('',*,*,#7854,.T.);
#10149=ORIENTED_EDGE('',*,*,#7857,.T.);
#10150=ORIENTED_EDGE('',*,*,#7860,.T.);
#10151=ORIENTED_EDGE('',*,*,#7863,.T.);
#10152=ORIENTED_EDGE('',*,*,#7866,.T.);
#10153=ORIENTED_EDGE('',*,*,#7910,.T.);
#10154=ORIENTED_EDGE('',*,*,#7906,.T.);
#10155=ORIENTED_EDGE('',*,*,#7813,.T.);
#10156=ORIENTED_EDGE('',*,*,#7817,.T.);
#10157=ORIENTED_EDGE('',*,*,#7820,.T.);
#10158=ORIENTED_EDGE('',*,*,#7823,.T.);
#10159=ORIENTED_EDGE('',*,*,#7826,.T.);
#10160=ORIENTED_EDGE('',*,*,#7829,.T.);
#10161=ORIENTED_EDGE('',*,*,#7832,.T.);
#10162=ORIENTED_EDGE('',*,*,#7835,.T.);
#10163=ORIENTED_EDGE('',*,*,#7838,.T.);
#10164=ORIENTED_EDGE('',*,*,#7905,.T.);
#10165=ORIENTED_EDGE('',*,*,#7901,.T.);
#10166=ORIENTED_EDGE('',*,*,#7897,.T.);
#10167=ORIENTED_EDGE('',*,*,#7783,.T.);
#10168=ORIENTED_EDGE('',*,*,#7903,.F.);
#10169=ORIENTED_EDGE('',*,*,#7904,.F.);
#10170=ORIENTED_EDGE('',*,*,#7836,.T.);
#10171=ORIENTED_EDGE('',*,*,#7833,.T.);
#10172=ORIENTED_EDGE('',*,*,#7830,.T.);
#10173=ORIENTED_EDGE('',*,*,#7827,.T.);
#10174=ORIENTED_EDGE('',*,*,#7824,.T.);
#10175=ORIENTED_EDGE('',*,*,#7821,.T.);
#10176=ORIENTED_EDGE('',*,*,#7818,.T.);
#10177=ORIENTED_EDGE('',*,*,#7815,.T.);
#10178=ORIENTED_EDGE('',*,*,#7811,.T.);
#10179=ORIENTED_EDGE('',*,*,#7908,.F.);
#10180=ORIENTED_EDGE('',*,*,#7909,.F.);
#10181=ORIENTED_EDGE('',*,*,#7864,.T.);
#10182=ORIENTED_EDGE('',*,*,#7861,.T.);
#10183=ORIENTED_EDGE('',*,*,#7858,.T.);
#10184=ORIENTED_EDGE('',*,*,#7855,.T.);
#10185=ORIENTED_EDGE('',*,*,#7852,.T.);
#10186=ORIENTED_EDGE('',*,*,#7849,.T.);
#10187=ORIENTED_EDGE('',*,*,#7846,.T.);
#10188=ORIENTED_EDGE('',*,*,#7843,.T.);
#10189=ORIENTED_EDGE('',*,*,#7839,.T.);
#10190=ORIENTED_EDGE('',*,*,#7913,.F.);
#10191=ORIENTED_EDGE('',*,*,#7914,.F.);
#10192=ORIENTED_EDGE('',*,*,#7892,.T.);
#10193=ORIENTED_EDGE('',*,*,#7889,.T.);
#10194=ORIENTED_EDGE('',*,*,#7886,.T.);
#10195=ORIENTED_EDGE('',*,*,#7883,.T.);
#10196=ORIENTED_EDGE('',*,*,#7880,.T.);
#10197=ORIENTED_EDGE('',*,*,#7877,.T.);
#10198=ORIENTED_EDGE('',*,*,#7874,.T.);
#10199=ORIENTED_EDGE('',*,*,#7871,.T.);
#10200=ORIENTED_EDGE('',*,*,#7867,.T.);
#10201=ORIENTED_EDGE('',*,*,#7917,.F.);
#10202=ORIENTED_EDGE('',*,*,#7898,.F.);
#10203=ORIENTED_EDGE('',*,*,#7808,.T.);
#10204=ORIENTED_EDGE('',*,*,#7805,.T.);
#10205=ORIENTED_EDGE('',*,*,#7802,.T.);
#10206=ORIENTED_EDGE('',*,*,#7799,.T.);
#10207=ORIENTED_EDGE('',*,*,#7796,.T.);
#10208=ORIENTED_EDGE('',*,*,#7793,.T.);
#10209=ORIENTED_EDGE('',*,*,#7790,.T.);
#10210=ORIENTED_EDGE('',*,*,#7787,.T.);
#10211=ORIENTED_EDGE('',*,*,#7895,.T.);
#10212=ORIENTED_EDGE('',*,*,#7918,.F.);
#10213=ORIENTED_EDGE('',*,*,#7919,.F.);
#10214=ORIENTED_EDGE('',*,*,#7920,.F.);
#10215=ORIENTED_EDGE('',*,*,#7921,.F.);
#10216=ORIENTED_EDGE('',*,*,#7920,.T.);
#10217=ORIENTED_EDGE('',*,*,#7922,.T.);
#10218=ORIENTED_EDGE('',*,*,#7923,.F.);
#10219=ORIENTED_EDGE('',*,*,#7924,.F.);
#10220=ORIENTED_EDGE('',*,*,#7925,.T.);
#10221=ORIENTED_EDGE('',*,*,#7926,.T.);
#10222=ORIENTED_EDGE('',*,*,#7927,.T.);
#10223=ORIENTED_EDGE('',*,*,#7923,.T.);
#10224=ORIENTED_EDGE('',*,*,#7928,.T.);
#10225=ORIENTED_EDGE('',*,*,#7925,.F.);
#10226=ORIENTED_EDGE('',*,*,#7922,.F.);
#10227=ORIENTED_EDGE('',*,*,#7919,.T.);
#10228=ORIENTED_EDGE('',*,*,#7929,.F.);
#10229=ORIENTED_EDGE('',*,*,#7930,.F.);
#10230=ORIENTED_EDGE('',*,*,#7931,.T.);
#10231=ORIENTED_EDGE('',*,*,#7932,.F.);
#10232=ORIENTED_EDGE('',*,*,#7933,.T.);
#10233=ORIENTED_EDGE('',*,*,#7934,.T.);
#10234=ORIENTED_EDGE('',*,*,#7935,.T.);
#10235=ORIENTED_EDGE('',*,*,#7936,.T.);
#10236=ORIENTED_EDGE('',*,*,#7937,.T.);
#10237=ORIENTED_EDGE('',*,*,#7926,.F.);
#10238=ORIENTED_EDGE('',*,*,#7935,.F.);
#10239=ORIENTED_EDGE('',*,*,#7938,.F.);
#10240=ORIENTED_EDGE('',*,*,#7939,.F.);
#10241=ORIENTED_EDGE('',*,*,#7936,.F.);
#10242=ORIENTED_EDGE('',*,*,#7934,.F.);
#10243=ORIENTED_EDGE('',*,*,#7927,.F.);
#10244=ORIENTED_EDGE('',*,*,#7937,.F.);
#10245=ORIENTED_EDGE('',*,*,#7939,.T.);
#10246=ORIENTED_EDGE('',*,*,#7940,.F.);
#10247=ORIENTED_EDGE('',*,*,#7941,.F.);
#10248=ORIENTED_EDGE('',*,*,#7942,.T.);
#10249=ORIENTED_EDGE('',*,*,#7943,.F.);
#10250=ORIENTED_EDGE('',*,*,#7944,.T.);
#10251=ORIENTED_EDGE('',*,*,#7921,.T.);
#10252=ORIENTED_EDGE('',*,*,#7924,.T.);
#10253=ORIENTED_EDGE('',*,*,#7938,.T.);
#10254=ORIENTED_EDGE('',*,*,#7933,.F.);
#10255=ORIENTED_EDGE('',*,*,#7945,.F.);
#10256=ORIENTED_EDGE('',*,*,#7940,.T.);
#10257=ORIENTED_EDGE('',*,*,#7941,.T.);
#10258=ORIENTED_EDGE('',*,*,#7945,.T.);
#10259=ORIENTED_EDGE('',*,*,#7932,.T.);
#10260=ORIENTED_EDGE('',*,*,#7946,.T.);
#10261=ORIENTED_EDGE('',*,*,#7947,.T.);
#10262=ORIENTED_EDGE('',*,*,#7948,.T.);
#10263=ORIENTED_EDGE('',*,*,#7947,.F.);
#10264=ORIENTED_EDGE('',*,*,#7949,.F.);
#10265=ORIENTED_EDGE('',*,*,#7950,.T.);
#10266=ORIENTED_EDGE('',*,*,#7928,.F.);
#10267=ORIENTED_EDGE('',*,*,#7950,.F.);
#10268=ORIENTED_EDGE('',*,*,#7951,.F.);
#10269=ORIENTED_EDGE('',*,*,#7952,.F.);
#10270=ORIENTED_EDGE('',*,*,#7953,.F.);
#10271=ORIENTED_EDGE('',*,*,#7946,.F.);
#10272=ORIENTED_EDGE('',*,*,#7931,.F.);
#10273=ORIENTED_EDGE('',*,*,#7954,.F.);
#10274=ORIENTED_EDGE('',*,*,#7951,.T.);
#10275=ORIENTED_EDGE('',*,*,#7949,.T.);
#10276=ORIENTED_EDGE('',*,*,#7948,.F.);
#10277=ORIENTED_EDGE('',*,*,#7953,.T.);
#10278=ORIENTED_EDGE('',*,*,#7955,.F.);
#10279=ORIENTED_EDGE('',*,*,#7942,.F.);
#10280=ORIENTED_EDGE('',*,*,#7930,.T.);
#10281=ORIENTED_EDGE('',*,*,#7956,.T.);
#10282=ORIENTED_EDGE('',*,*,#7943,.T.);
#10283=ORIENTED_EDGE('',*,*,#7955,.T.);
#10284=ORIENTED_EDGE('',*,*,#7952,.T.);
#10285=ORIENTED_EDGE('',*,*,#7954,.T.);
#10286=ORIENTED_EDGE('',*,*,#7918,.T.);
#10287=ORIENTED_EDGE('',*,*,#7944,.F.);
#10288=ORIENTED_EDGE('',*,*,#7956,.F.);
#10289=ORIENTED_EDGE('',*,*,#7929,.T.);
#10290=ORIENTED_EDGE('',*,*,#7957,.T.);
#10291=ORIENTED_EDGE('',*,*,#7958,.T.);
#10292=ORIENTED_EDGE('',*,*,#7959,.T.);
#10293=ORIENTED_EDGE('',*,*,#7958,.F.);
#10294=ORIENTED_EDGE('',*,*,#7959,.F.);
#10295=ORIENTED_EDGE('',*,*,#7960,.T.);
#10296=ORIENTED_EDGE('',*,*,#7961,.T.);
#10297=ORIENTED_EDGE('',*,*,#7960,.F.);
#10298=ORIENTED_EDGE('',*,*,#7962,.T.);
#10299=ORIENTED_EDGE('',*,*,#7957,.F.);
#10300=ORIENTED_EDGE('',*,*,#7962,.F.);
#10301=ORIENTED_EDGE('',*,*,#7963,.T.);
#10302=ORIENTED_EDGE('',*,*,#7964,.T.);
#10303=ORIENTED_EDGE('',*,*,#7963,.F.);
#10304=ORIENTED_EDGE('',*,*,#7964,.F.);
#10305=ORIENTED_EDGE('',*,*,#7961,.F.);
#10306=ORIENTED_EDGE('',*,*,#7965,.F.);
#10307=ORIENTED_EDGE('',*,*,#7966,.T.);
#10308=ORIENTED_EDGE('',*,*,#7967,.F.);
#10309=ORIENTED_EDGE('',*,*,#7966,.F.);
#10310=ORIENTED_EDGE('',*,*,#7965,.T.);
#10311=ORIENTED_EDGE('',*,*,#7968,.F.);
#10312=ORIENTED_EDGE('',*,*,#7969,.F.);
#10313=ORIENTED_EDGE('',*,*,#7970,.T.);
#10314=ORIENTED_EDGE('',*,*,#7971,.F.);
#10315=ORIENTED_EDGE('',*,*,#7970,.F.);
#10316=ORIENTED_EDGE('',*,*,#7969,.T.);
#10317=ORIENTED_EDGE('',*,*,#7972,.F.);
#10318=ORIENTED_EDGE('',*,*,#7973,.F.);
#10319=ORIENTED_EDGE('',*,*,#7974,.T.);
#10320=ORIENTED_EDGE('',*,*,#7975,.F.);
#10321=ORIENTED_EDGE('',*,*,#7974,.F.);
#10322=ORIENTED_EDGE('',*,*,#7973,.T.);
#10323=ORIENTED_EDGE('',*,*,#7976,.F.);
#10324=ORIENTED_EDGE('',*,*,#7977,.F.);
#10325=ORIENTED_EDGE('',*,*,#7978,.T.);
#10326=ORIENTED_EDGE('',*,*,#7979,.F.);
#10327=ORIENTED_EDGE('',*,*,#7978,.F.);
#10328=ORIENTED_EDGE('',*,*,#7977,.T.);
#10329=ORIENTED_EDGE('',*,*,#7980,.F.);
#10330=ORIENTED_EDGE('',*,*,#7981,.F.);
#10331=ORIENTED_EDGE('',*,*,#7982,.T.);
#10332=ORIENTED_EDGE('',*,*,#7968,.T.);
#10333=ORIENTED_EDGE('',*,*,#7982,.F.);
#10334=ORIENTED_EDGE('',*,*,#7983,.F.);
#10335=ORIENTED_EDGE('',*,*,#7984,.T.);
#10336=ORIENTED_EDGE('',*,*,#7972,.T.);
#10337=ORIENTED_EDGE('',*,*,#7984,.F.);
#10338=ORIENTED_EDGE('',*,*,#7985,.F.);
#10339=ORIENTED_EDGE('',*,*,#7986,.T.);
#10340=ORIENTED_EDGE('',*,*,#7976,.T.);
#10341=ORIENTED_EDGE('',*,*,#7986,.F.);
#10342=ORIENTED_EDGE('',*,*,#7987,.F.);
#10343=ORIENTED_EDGE('',*,*,#7988,.T.);
#10344=ORIENTED_EDGE('',*,*,#7980,.T.);
#10345=ORIENTED_EDGE('',*,*,#7988,.F.);
#10346=ORIENTED_EDGE('',*,*,#7989,.T.);
#10347=ORIENTED_EDGE('',*,*,#7990,.T.);
#10348=ORIENTED_EDGE('',*,*,#7991,.F.);
#10349=ORIENTED_EDGE('',*,*,#7992,.F.);
#10350=ORIENTED_EDGE('',*,*,#7993,.T.);
#10351=ORIENTED_EDGE('',*,*,#7992,.T.);
#10352=ORIENTED_EDGE('',*,*,#7994,.F.);
#10353=ORIENTED_EDGE('',*,*,#7995,.F.);
#10354=ORIENTED_EDGE('',*,*,#7996,.T.);
#10355=ORIENTED_EDGE('',*,*,#7995,.T.);
#10356=ORIENTED_EDGE('',*,*,#7997,.F.);
#10357=ORIENTED_EDGE('',*,*,#7998,.F.);
#10358=ORIENTED_EDGE('',*,*,#7999,.T.);
#10359=ORIENTED_EDGE('',*,*,#7998,.T.);
#10360=ORIENTED_EDGE('',*,*,#8000,.F.);
#10361=ORIENTED_EDGE('',*,*,#8001,.F.);
#10362=ORIENTED_EDGE('',*,*,#8002,.T.);
#10363=ORIENTED_EDGE('',*,*,#8001,.T.);
#10364=ORIENTED_EDGE('',*,*,#8003,.F.);
#10365=ORIENTED_EDGE('',*,*,#8004,.F.);
#10366=ORIENTED_EDGE('',*,*,#7979,.T.);
#10367=ORIENTED_EDGE('',*,*,#7975,.T.);
#10368=ORIENTED_EDGE('',*,*,#7971,.T.);
#10369=ORIENTED_EDGE('',*,*,#7967,.T.);
#10370=ORIENTED_EDGE('',*,*,#8005,.T.);
#10371=ORIENTED_EDGE('',*,*,#8004,.T.);
#10372=ORIENTED_EDGE('',*,*,#8006,.F.);
#10373=ORIENTED_EDGE('',*,*,#8007,.F.);
#10374=ORIENTED_EDGE('',*,*,#8008,.T.);
#10375=ORIENTED_EDGE('',*,*,#8007,.T.);
#10376=ORIENTED_EDGE('',*,*,#8009,.F.);
#10377=ORIENTED_EDGE('',*,*,#8010,.F.);
#10378=ORIENTED_EDGE('',*,*,#8011,.T.);
#10379=ORIENTED_EDGE('',*,*,#8010,.T.);
#10380=ORIENTED_EDGE('',*,*,#8012,.F.);
#10381=ORIENTED_EDGE('',*,*,#8013,.F.);
#10382=ORIENTED_EDGE('',*,*,#8014,.T.);
#10383=ORIENTED_EDGE('',*,*,#8013,.T.);
#10384=ORIENTED_EDGE('',*,*,#8015,.F.);
#10385=ORIENTED_EDGE('',*,*,#8016,.F.);
#10386=ORIENTED_EDGE('',*,*,#8017,.T.);
#10387=ORIENTED_EDGE('',*,*,#8016,.T.);
#10388=ORIENTED_EDGE('',*,*,#8018,.F.);
#10389=ORIENTED_EDGE('',*,*,#8019,.F.);
#10390=ORIENTED_EDGE('',*,*,#8020,.T.);
#10391=ORIENTED_EDGE('',*,*,#8019,.T.);
#10392=ORIENTED_EDGE('',*,*,#8021,.F.);
#10393=ORIENTED_EDGE('',*,*,#8022,.F.);
#10394=ORIENTED_EDGE('',*,*,#7981,.T.);
#10395=ORIENTED_EDGE('',*,*,#7983,.T.);
#10396=ORIENTED_EDGE('',*,*,#7985,.T.);
#10397=ORIENTED_EDGE('',*,*,#7987,.T.);
#10398=ORIENTED_EDGE('',*,*,#8023,.T.);
#10399=ORIENTED_EDGE('',*,*,#8022,.T.);
#10400=ORIENTED_EDGE('',*,*,#8024,.F.);
#10401=ORIENTED_EDGE('',*,*,#7990,.F.);
#10402=ORIENTED_EDGE('',*,*,#8024,.T.);
#10403=ORIENTED_EDGE('',*,*,#8021,.T.);
#10404=ORIENTED_EDGE('',*,*,#8018,.T.);
#10405=ORIENTED_EDGE('',*,*,#8015,.T.);
#10406=ORIENTED_EDGE('',*,*,#8012,.T.);
#10407=ORIENTED_EDGE('',*,*,#8009,.T.);
#10408=ORIENTED_EDGE('',*,*,#8006,.T.);
#10409=ORIENTED_EDGE('',*,*,#8003,.T.);
#10410=ORIENTED_EDGE('',*,*,#8000,.T.);
#10411=ORIENTED_EDGE('',*,*,#7997,.T.);
#10412=ORIENTED_EDGE('',*,*,#7994,.T.);
#10413=ORIENTED_EDGE('',*,*,#7991,.T.);
#10414=ORIENTED_EDGE('',*,*,#8023,.F.);
#10415=ORIENTED_EDGE('',*,*,#7989,.F.);
#10416=ORIENTED_EDGE('',*,*,#7993,.F.);
#10417=ORIENTED_EDGE('',*,*,#7996,.F.);
#10418=ORIENTED_EDGE('',*,*,#7999,.F.);
#10419=ORIENTED_EDGE('',*,*,#8002,.F.);
#10420=ORIENTED_EDGE('',*,*,#8005,.F.);
#10421=ORIENTED_EDGE('',*,*,#8008,.F.);
#10422=ORIENTED_EDGE('',*,*,#8011,.F.);
#10423=ORIENTED_EDGE('',*,*,#8014,.F.);
#10424=ORIENTED_EDGE('',*,*,#8017,.F.);
#10425=ORIENTED_EDGE('',*,*,#8020,.F.);
#10426=ORIENTED_EDGE('',*,*,#8025,.F.);
#10427=ORIENTED_EDGE('',*,*,#8026,.F.);
#10428=ORIENTED_EDGE('',*,*,#8027,.T.);
#10429=ORIENTED_EDGE('',*,*,#8025,.T.);
#10430=ORIENTED_EDGE('',*,*,#8027,.F.);
#10431=ORIENTED_EDGE('',*,*,#8028,.F.);
#10432=ORIENTED_EDGE('',*,*,#8029,.T.);
#10433=ORIENTED_EDGE('',*,*,#8026,.T.);
#10434=ORIENTED_EDGE('',*,*,#8029,.F.);
#10435=ORIENTED_EDGE('',*,*,#8030,.F.);
#10436=ORIENTED_EDGE('',*,*,#8031,.T.);
#10437=ORIENTED_EDGE('',*,*,#8028,.T.);
#10438=ORIENTED_EDGE('',*,*,#8031,.F.);
#10439=ORIENTED_EDGE('',*,*,#8030,.T.);
#10440=ORIENTED_EDGE('',*,*,#8032,.F.);
#10441=ORIENTED_EDGE('',*,*,#8033,.F.);
#10442=ORIENTED_EDGE('',*,*,#8034,.T.);
#10443=ORIENTED_EDGE('',*,*,#8032,.T.);
#10444=ORIENTED_EDGE('',*,*,#8034,.F.);
#10445=ORIENTED_EDGE('',*,*,#8035,.F.);
#10446=ORIENTED_EDGE('',*,*,#8036,.T.);
#10447=ORIENTED_EDGE('',*,*,#8033,.T.);
#10448=ORIENTED_EDGE('',*,*,#8036,.F.);
#10449=ORIENTED_EDGE('',*,*,#8037,.F.);
#10450=ORIENTED_EDGE('',*,*,#8038,.T.);
#10451=ORIENTED_EDGE('',*,*,#8035,.T.);
#10452=ORIENTED_EDGE('',*,*,#8038,.F.);
#10453=ORIENTED_EDGE('',*,*,#8037,.T.);
#10454=ORIENTED_EDGE('',*,*,#8039,.T.);
#10455=ORIENTED_EDGE('',*,*,#8040,.T.);
#10456=ORIENTED_EDGE('',*,*,#8041,.T.);
#10457=ORIENTED_EDGE('',*,*,#8042,.F.);
#10458=ORIENTED_EDGE('',*,*,#8043,.T.);
#10459=ORIENTED_EDGE('',*,*,#8044,.T.);
#10460=ORIENTED_EDGE('',*,*,#8045,.T.);
#10461=ORIENTED_EDGE('',*,*,#8040,.F.);
#10462=ORIENTED_EDGE('',*,*,#8046,.T.);
#10463=ORIENTED_EDGE('',*,*,#8047,.T.);
#10464=ORIENTED_EDGE('',*,*,#8048,.T.);
#10465=ORIENTED_EDGE('',*,*,#8044,.F.);
#10466=ORIENTED_EDGE('',*,*,#8049,.T.);
#10467=ORIENTED_EDGE('',*,*,#8050,.T.);
#10468=ORIENTED_EDGE('',*,*,#8051,.T.);
#10469=ORIENTED_EDGE('',*,*,#8047,.F.);
#10470=ORIENTED_EDGE('',*,*,#8052,.T.);
#10471=ORIENTED_EDGE('',*,*,#8053,.T.);
#10472=ORIENTED_EDGE('',*,*,#8054,.T.);
#10473=ORIENTED_EDGE('',*,*,#8050,.F.);
#10474=ORIENTED_EDGE('',*,*,#8055,.T.);
#10475=ORIENTED_EDGE('',*,*,#8042,.T.);
#10476=ORIENTED_EDGE('',*,*,#8056,.T.);
#10477=ORIENTED_EDGE('',*,*,#8053,.F.);
#10478=ORIENTED_EDGE('',*,*,#8055,.F.);
#10479=ORIENTED_EDGE('',*,*,#8052,.F.);
#10480=ORIENTED_EDGE('',*,*,#8049,.F.);
#10481=ORIENTED_EDGE('',*,*,#8046,.F.);
#10482=ORIENTED_EDGE('',*,*,#8043,.F.);
#10483=ORIENTED_EDGE('',*,*,#8039,.F.);
#10484=ORIENTED_EDGE('',*,*,#8056,.F.);
#10485=ORIENTED_EDGE('',*,*,#8041,.F.);
#10486=ORIENTED_EDGE('',*,*,#8045,.F.);
#10487=ORIENTED_EDGE('',*,*,#8048,.F.);
#10488=ORIENTED_EDGE('',*,*,#8051,.F.);
#10489=ORIENTED_EDGE('',*,*,#8054,.F.);
#10490=ORIENTED_EDGE('',*,*,#8057,.F.);
#10491=ORIENTED_EDGE('',*,*,#8058,.F.);
#10492=ORIENTED_EDGE('',*,*,#8059,.T.);
#10493=ORIENTED_EDGE('',*,*,#8060,.F.);
#10494=ORIENTED_EDGE('',*,*,#8061,.F.);
#10495=ORIENTED_EDGE('',*,*,#8059,.F.);
#10496=ORIENTED_EDGE('',*,*,#8060,.T.);
#10497=ORIENTED_EDGE('',*,*,#8061,.T.);
#10498=ORIENTED_EDGE('',*,*,#8062,.T.);
#10499=ORIENTED_EDGE('',*,*,#8063,.T.);
#10500=ORIENTED_EDGE('',*,*,#8062,.F.);
#10501=ORIENTED_EDGE('',*,*,#8064,.T.);
#10502=ORIENTED_EDGE('',*,*,#8065,.T.);
#10503=ORIENTED_EDGE('',*,*,#8066,.F.);
#10504=ORIENTED_EDGE('',*,*,#8065,.F.);
#10505=ORIENTED_EDGE('',*,*,#8066,.T.);
#10506=ORIENTED_EDGE('',*,*,#8067,.T.);
#10507=ORIENTED_EDGE('',*,*,#8068,.F.);
#10508=ORIENTED_EDGE('',*,*,#8067,.F.);
#10509=ORIENTED_EDGE('',*,*,#8063,.F.);
#10510=ORIENTED_EDGE('',*,*,#8068,.T.);
#10511=ORIENTED_EDGE('',*,*,#8069,.F.);
#10512=ORIENTED_EDGE('',*,*,#8070,.T.);
#10513=ORIENTED_EDGE('',*,*,#8057,.T.);
#10514=ORIENTED_EDGE('',*,*,#8058,.T.);
#10515=ORIENTED_EDGE('',*,*,#8070,.F.);
#10516=ORIENTED_EDGE('',*,*,#8069,.T.);
#10517=ORIENTED_EDGE('',*,*,#8071,.F.);
#10518=ORIENTED_EDGE('',*,*,#8071,.T.);
#10519=ORIENTED_EDGE('',*,*,#8072,.T.);
#10520=ORIENTED_EDGE('',*,*,#8064,.F.);
#10521=ORIENTED_EDGE('',*,*,#8072,.F.);
#10522=ORIENTED_EDGE('',*,*,#8073,.F.);
#10523=ORIENTED_EDGE('',*,*,#8074,.F.);
#10524=ORIENTED_EDGE('',*,*,#8075,.T.);
#10525=ORIENTED_EDGE('',*,*,#8076,.F.);
#10526=ORIENTED_EDGE('',*,*,#8077,.F.);
#10527=ORIENTED_EDGE('',*,*,#8075,.F.);
#10528=ORIENTED_EDGE('',*,*,#8078,.T.);
#10529=ORIENTED_EDGE('',*,*,#8079,.T.);
#10530=ORIENTED_EDGE('',*,*,#8076,.T.);
#10531=ORIENTED_EDGE('',*,*,#8077,.T.);
#10532=ORIENTED_EDGE('',*,*,#8079,.F.);
#10533=ORIENTED_EDGE('',*,*,#8080,.F.);
#10534=ORIENTED_EDGE('',*,*,#8081,.T.);
#10535=ORIENTED_EDGE('',*,*,#8082,.F.);
#10536=ORIENTED_EDGE('',*,*,#8083,.T.);
#10537=ORIENTED_EDGE('',*,*,#8080,.T.);
#10538=ORIENTED_EDGE('',*,*,#8083,.F.);
#10539=ORIENTED_EDGE('',*,*,#8084,.F.);
#10540=ORIENTED_EDGE('',*,*,#8085,.T.);
#10541=ORIENTED_EDGE('',*,*,#8082,.T.);
#10542=ORIENTED_EDGE('',*,*,#8085,.F.);
#10543=ORIENTED_EDGE('',*,*,#8086,.F.);
#10544=ORIENTED_EDGE('',*,*,#8087,.T.);
#10545=ORIENTED_EDGE('',*,*,#8084,.T.);
#10546=ORIENTED_EDGE('',*,*,#8087,.F.);
#10547=ORIENTED_EDGE('',*,*,#8086,.T.);
#10548=ORIENTED_EDGE('',*,*,#8078,.F.);
#10549=ORIENTED_EDGE('',*,*,#8073,.T.);
#10550=ORIENTED_EDGE('',*,*,#8074,.T.);
#10551=ORIENTED_EDGE('',*,*,#8088,.T.);
#10552=ORIENTED_EDGE('',*,*,#8081,.F.);
#10553=ORIENTED_EDGE('',*,*,#8088,.F.);
#10554=ORIENTED_EDGE('',*,*,#8089,.T.);
#10555=ORIENTED_EDGE('',*,*,#8089,.F.);
#10556=ORIENTED_EDGE('',*,*,#8090,.T.);
#10557=ORIENTED_EDGE('',*,*,#8090,.F.);
#10558=ORIENTED_EDGE('',*,*,#8091,.T.);
#10559=ORIENTED_EDGE('',*,*,#8091,.F.);
#10560=ORIENTED_EDGE('',*,*,#8092,.T.);
#10561=ORIENTED_EDGE('',*,*,#8092,.F.);
#10562=ORIENTED_EDGE('',*,*,#8093,.T.);
#10563=ORIENTED_EDGE('',*,*,#8093,.F.);
#10564=ORIENTED_EDGE('',*,*,#8094,.T.);
#10565=ORIENTED_EDGE('',*,*,#8094,.F.);
#10566=ORIENTED_EDGE('',*,*,#8095,.T.);
#10567=ORIENTED_EDGE('',*,*,#8095,.F.);
#10568=ORIENTED_EDGE('',*,*,#8096,.F.);
#10569=ORIENTED_EDGE('',*,*,#8097,.F.);
#10570=ORIENTED_EDGE('',*,*,#8098,.F.);
#10571=ORIENTED_EDGE('',*,*,#8099,.F.);
#10572=ORIENTED_EDGE('',*,*,#8098,.T.);
#10573=ORIENTED_EDGE('',*,*,#8100,.F.);
#10574=ORIENTED_EDGE('',*,*,#8101,.T.);
#10575=ORIENTED_EDGE('',*,*,#8102,.F.);
#10576=ORIENTED_EDGE('',*,*,#8103,.T.);
#10577=ORIENTED_EDGE('',*,*,#8104,.F.);
#10578=ORIENTED_EDGE('',*,*,#8105,.T.);
#10579=ORIENTED_EDGE('',*,*,#8106,.F.);
#10580=ORIENTED_EDGE('',*,*,#8105,.F.);
#10581=ORIENTED_EDGE('',*,*,#8107,.F.);
#10582=ORIENTED_EDGE('',*,*,#8108,.T.);
#10583=ORIENTED_EDGE('',*,*,#8109,.F.);
#10584=ORIENTED_EDGE('',*,*,#8110,.T.);
#10585=ORIENTED_EDGE('',*,*,#8111,.F.);
#10586=ORIENTED_EDGE('',*,*,#8112,.T.);
#10587=ORIENTED_EDGE('',*,*,#8113,.F.);
#10588=ORIENTED_EDGE('',*,*,#8114,.T.);
#10589=ORIENTED_EDGE('',*,*,#8115,.F.);
#10590=ORIENTED_EDGE('',*,*,#8097,.T.);
#10591=ORIENTED_EDGE('',*,*,#8116,.T.);
#10592=ORIENTED_EDGE('',*,*,#8117,.T.);
#10593=ORIENTED_EDGE('',*,*,#8100,.T.);
#10594=ORIENTED_EDGE('',*,*,#8118,.F.);
#10595=ORIENTED_EDGE('',*,*,#8119,.F.);
#10596=ORIENTED_EDGE('',*,*,#8101,.F.);
#10597=ORIENTED_EDGE('',*,*,#8117,.F.);
#10598=ORIENTED_EDGE('',*,*,#8119,.T.);
#10599=ORIENTED_EDGE('',*,*,#8120,.T.);
#10600=ORIENTED_EDGE('',*,*,#8121,.T.);
#10601=ORIENTED_EDGE('',*,*,#8102,.T.);
#10602=ORIENTED_EDGE('',*,*,#8122,.F.);
#10603=ORIENTED_EDGE('',*,*,#8123,.F.);
#10604=ORIENTED_EDGE('',*,*,#8103,.F.);
#10605=ORIENTED_EDGE('',*,*,#8121,.F.);
#10606=ORIENTED_EDGE('',*,*,#8123,.T.);
#10607=ORIENTED_EDGE('',*,*,#8124,.T.);
#10608=ORIENTED_EDGE('',*,*,#8125,.T.);
#10609=ORIENTED_EDGE('',*,*,#8126,.T.);
#10610=ORIENTED_EDGE('',*,*,#8107,.T.);
#10611=ORIENTED_EDGE('',*,*,#8104,.T.);
#10612=ORIENTED_EDGE('',*,*,#8127,.F.);
#10613=ORIENTED_EDGE('',*,*,#8128,.F.);
#10614=ORIENTED_EDGE('',*,*,#8108,.F.);
#10615=ORIENTED_EDGE('',*,*,#8126,.F.);
#10616=ORIENTED_EDGE('',*,*,#8128,.T.);
#10617=ORIENTED_EDGE('',*,*,#8129,.T.);
#10618=ORIENTED_EDGE('',*,*,#8130,.T.);
#10619=ORIENTED_EDGE('',*,*,#8109,.T.);
#10620=ORIENTED_EDGE('',*,*,#8131,.F.);
#10621=ORIENTED_EDGE('',*,*,#8132,.F.);
#10622=ORIENTED_EDGE('',*,*,#8110,.F.);
#10623=ORIENTED_EDGE('',*,*,#8130,.F.);
#10624=ORIENTED_EDGE('',*,*,#8132,.T.);
#10625=ORIENTED_EDGE('',*,*,#8133,.T.);
#10626=ORIENTED_EDGE('',*,*,#8134,.T.);
#10627=ORIENTED_EDGE('',*,*,#8111,.T.);
#10628=ORIENTED_EDGE('',*,*,#8112,.F.);
#10629=ORIENTED_EDGE('',*,*,#8134,.F.);
#10630=ORIENTED_EDGE('',*,*,#8135,.F.);
#10631=ORIENTED_EDGE('',*,*,#8136,.F.);
#10632=ORIENTED_EDGE('',*,*,#8137,.F.);
#10633=ORIENTED_EDGE('',*,*,#8138,.T.);
#10634=ORIENTED_EDGE('',*,*,#8124,.F.);
#10635=ORIENTED_EDGE('',*,*,#8122,.T.);
#10636=ORIENTED_EDGE('',*,*,#8120,.F.);
#10637=ORIENTED_EDGE('',*,*,#8118,.T.);
#10638=ORIENTED_EDGE('',*,*,#8116,.F.);
#10639=ORIENTED_EDGE('',*,*,#8096,.T.);
#10640=ORIENTED_EDGE('',*,*,#8139,.F.);
#10641=ORIENTED_EDGE('',*,*,#8140,.T.);
#10642=ORIENTED_EDGE('',*,*,#8141,.F.);
#10643=ORIENTED_EDGE('',*,*,#8135,.T.);
#10644=ORIENTED_EDGE('',*,*,#8133,.F.);
#10645=ORIENTED_EDGE('',*,*,#8131,.T.);
#10646=ORIENTED_EDGE('',*,*,#8129,.F.);
#10647=ORIENTED_EDGE('',*,*,#8127,.T.);
#10648=ORIENTED_EDGE('',*,*,#8125,.F.);
#10649=ORIENTED_EDGE('',*,*,#8138,.F.);
#10650=ORIENTED_EDGE('',*,*,#8099,.T.);
#10651=ORIENTED_EDGE('',*,*,#8115,.T.);
#10652=ORIENTED_EDGE('',*,*,#8142,.T.);
#10653=ORIENTED_EDGE('',*,*,#8139,.T.);
#10654=ORIENTED_EDGE('',*,*,#8114,.F.);
#10655=ORIENTED_EDGE('',*,*,#8143,.F.);
#10656=ORIENTED_EDGE('',*,*,#8140,.F.);
#10657=ORIENTED_EDGE('',*,*,#8142,.F.);
#10658=ORIENTED_EDGE('',*,*,#8106,.T.);
#10659=ORIENTED_EDGE('',*,*,#8137,.T.);
#10660=ORIENTED_EDGE('',*,*,#8136,.T.);
#10661=ORIENTED_EDGE('',*,*,#8141,.T.);
#10662=ORIENTED_EDGE('',*,*,#8143,.T.);
#10663=ORIENTED_EDGE('',*,*,#8113,.T.);
#10664=ORIENTED_EDGE('',*,*,#8144,.F.);
#10665=ORIENTED_EDGE('',*,*,#8145,.T.);
#10666=ORIENTED_EDGE('',*,*,#8146,.F.);
#10667=ORIENTED_EDGE('',*,*,#8147,.T.);
#10668=ORIENTED_EDGE('',*,*,#8144,.T.);
#10669=ORIENTED_EDGE('',*,*,#8147,.F.);
#10670=ORIENTED_EDGE('',*,*,#8146,.T.);
#10671=ORIENTED_EDGE('',*,*,#8148,.F.);
#10672=ORIENTED_EDGE('',*,*,#8148,.T.);
#10673=ORIENTED_EDGE('',*,*,#8149,.T.);
#10674=ORIENTED_EDGE('',*,*,#8145,.F.);
#10675=ORIENTED_EDGE('',*,*,#8149,.F.);
#10676=ORIENTED_EDGE('',*,*,#8150,.F.);
#10677=ORIENTED_EDGE('',*,*,#8151,.T.);
#10678=ORIENTED_EDGE('',*,*,#8152,.F.);
#10679=ORIENTED_EDGE('',*,*,#8153,.T.);
#10680=ORIENTED_EDGE('',*,*,#8150,.T.);
#10681=ORIENTED_EDGE('',*,*,#8153,.F.);
#10682=ORIENTED_EDGE('',*,*,#8152,.T.);
#10683=ORIENTED_EDGE('',*,*,#8154,.F.);
#10684=ORIENTED_EDGE('',*,*,#8154,.T.);
#10685=ORIENTED_EDGE('',*,*,#8155,.T.);
#10686=ORIENTED_EDGE('',*,*,#8151,.F.);
#10687=ORIENTED_EDGE('',*,*,#8155,.F.);
#10688=ORIENTED_EDGE('',*,*,#8156,.T.);
#10689=ORIENTED_EDGE('',*,*,#8157,.T.);
#10690=ORIENTED_EDGE('',*,*,#8158,.T.);
#10691=ORIENTED_EDGE('',*,*,#8159,.F.);
#10692=ORIENTED_EDGE('',*,*,#8160,.T.);
#10693=ORIENTED_EDGE('',*,*,#8161,.T.);
#10694=ORIENTED_EDGE('',*,*,#8162,.T.);
#10695=ORIENTED_EDGE('',*,*,#8157,.F.);
#10696=ORIENTED_EDGE('',*,*,#8163,.T.);
#10697=ORIENTED_EDGE('',*,*,#8164,.T.);
#10698=ORIENTED_EDGE('',*,*,#8165,.T.);
#10699=ORIENTED_EDGE('',*,*,#8161,.F.);
#10700=ORIENTED_EDGE('',*,*,#8166,.T.);
#10701=ORIENTED_EDGE('',*,*,#8167,.T.);
#10702=ORIENTED_EDGE('',*,*,#8168,.T.);
#10703=ORIENTED_EDGE('',*,*,#8164,.F.);
#10704=ORIENTED_EDGE('',*,*,#8169,.T.);
#10705=ORIENTED_EDGE('',*,*,#8170,.T.);
#10706=ORIENTED_EDGE('',*,*,#8171,.T.);
#10707=ORIENTED_EDGE('',*,*,#8167,.F.);
#10708=ORIENTED_EDGE('',*,*,#8172,.T.);
#10709=ORIENTED_EDGE('',*,*,#8159,.T.);
#10710=ORIENTED_EDGE('',*,*,#8173,.T.);
#10711=ORIENTED_EDGE('',*,*,#8170,.F.);
#10712=ORIENTED_EDGE('',*,*,#8172,.F.);
#10713=ORIENTED_EDGE('',*,*,#8169,.F.);
#10714=ORIENTED_EDGE('',*,*,#8166,.F.);
#10715=ORIENTED_EDGE('',*,*,#8163,.F.);
#10716=ORIENTED_EDGE('',*,*,#8160,.F.);
#10717=ORIENTED_EDGE('',*,*,#8156,.F.);
#10718=ORIENTED_EDGE('',*,*,#8173,.F.);
#10719=ORIENTED_EDGE('',*,*,#8158,.F.);
#10720=ORIENTED_EDGE('',*,*,#8162,.F.);
#10721=ORIENTED_EDGE('',*,*,#8165,.F.);
#10722=ORIENTED_EDGE('',*,*,#8168,.F.);
#10723=ORIENTED_EDGE('',*,*,#8171,.F.);
#10724=ORIENTED_EDGE('',*,*,#8174,.F.);
#10725=ORIENTED_EDGE('',*,*,#8175,.F.);
#10726=ORIENTED_EDGE('',*,*,#8176,.F.);
#10727=ORIENTED_EDGE('',*,*,#8177,.T.);
#10728=ORIENTED_EDGE('',*,*,#8175,.T.);
#10729=ORIENTED_EDGE('',*,*,#8177,.F.);
#10730=ORIENTED_EDGE('',*,*,#8178,.F.);
#10731=ORIENTED_EDGE('',*,*,#8179,.T.);
#10732=ORIENTED_EDGE('',*,*,#8176,.T.);
#10733=ORIENTED_EDGE('',*,*,#8179,.F.);
#10734=ORIENTED_EDGE('',*,*,#8180,.F.);
#10735=ORIENTED_EDGE('',*,*,#8181,.T.);
#10736=ORIENTED_EDGE('',*,*,#8178,.T.);
#10737=ORIENTED_EDGE('',*,*,#8181,.F.);
#10738=ORIENTED_EDGE('',*,*,#8180,.T.);
#10739=ORIENTED_EDGE('',*,*,#8182,.F.);
#10740=ORIENTED_EDGE('',*,*,#8183,.F.);
#10741=ORIENTED_EDGE('',*,*,#8184,.T.);
#10742=ORIENTED_EDGE('',*,*,#8182,.T.);
#10743=ORIENTED_EDGE('',*,*,#8184,.F.);
#10744=ORIENTED_EDGE('',*,*,#8174,.T.);
#10745=ORIENTED_EDGE('',*,*,#8185,.T.);
#10746=ORIENTED_EDGE('',*,*,#8183,.T.);
#10747=ORIENTED_EDGE('',*,*,#8185,.F.);
#10748=ORIENTED_EDGE('',*,*,#8186,.F.);
#10749=ORIENTED_EDGE('',*,*,#8187,.T.);
#10750=ORIENTED_EDGE('',*,*,#8188,.F.);
#10751=ORIENTED_EDGE('',*,*,#8187,.F.);
#10752=ORIENTED_EDGE('',*,*,#8189,.F.);
#10753=ORIENTED_EDGE('',*,*,#8190,.T.);
#10754=ORIENTED_EDGE('',*,*,#8191,.F.);
#10755=ORIENTED_EDGE('',*,*,#8190,.F.);
#10756=ORIENTED_EDGE('',*,*,#8192,.F.);
#10757=ORIENTED_EDGE('',*,*,#8193,.T.);
#10758=ORIENTED_EDGE('',*,*,#8194,.F.);
#10759=ORIENTED_EDGE('',*,*,#8193,.F.);
#10760=ORIENTED_EDGE('',*,*,#8195,.F.);
#10761=ORIENTED_EDGE('',*,*,#8196,.T.);
#10762=ORIENTED_EDGE('',*,*,#8197,.F.);
#10763=ORIENTED_EDGE('',*,*,#8196,.F.);
#10764=ORIENTED_EDGE('',*,*,#8198,.F.);
#10765=ORIENTED_EDGE('',*,*,#8199,.T.);
#10766=ORIENTED_EDGE('',*,*,#8200,.F.);
#10767=ORIENTED_EDGE('',*,*,#8199,.F.);
#10768=ORIENTED_EDGE('',*,*,#8201,.F.);
#10769=ORIENTED_EDGE('',*,*,#8202,.T.);
#10770=ORIENTED_EDGE('',*,*,#8203,.F.);
#10771=ORIENTED_EDGE('',*,*,#8202,.F.);
#10772=ORIENTED_EDGE('',*,*,#8204,.F.);
#10773=ORIENTED_EDGE('',*,*,#8205,.T.);
#10774=ORIENTED_EDGE('',*,*,#8206,.F.);
#10775=ORIENTED_EDGE('',*,*,#8205,.F.);
#10776=ORIENTED_EDGE('',*,*,#8207,.F.);
#10777=ORIENTED_EDGE('',*,*,#8208,.T.);
#10778=ORIENTED_EDGE('',*,*,#8209,.F.);
#10779=ORIENTED_EDGE('',*,*,#8208,.F.);
#10780=ORIENTED_EDGE('',*,*,#8210,.T.);
#10781=ORIENTED_EDGE('',*,*,#8211,.T.);
#10782=ORIENTED_EDGE('',*,*,#8212,.F.);
#10783=ORIENTED_EDGE('',*,*,#8213,.F.);
#10784=ORIENTED_EDGE('',*,*,#8214,.T.);
#10785=ORIENTED_EDGE('',*,*,#8213,.T.);
#10786=ORIENTED_EDGE('',*,*,#8215,.F.);
#10787=ORIENTED_EDGE('',*,*,#8216,.F.);
#10788=ORIENTED_EDGE('',*,*,#8217,.T.);
#10789=ORIENTED_EDGE('',*,*,#8216,.T.);
#10790=ORIENTED_EDGE('',*,*,#8218,.F.);
#10791=ORIENTED_EDGE('',*,*,#8219,.F.);
#10792=ORIENTED_EDGE('',*,*,#8220,.T.);
#10793=ORIENTED_EDGE('',*,*,#8219,.T.);
#10794=ORIENTED_EDGE('',*,*,#8221,.F.);
#10795=ORIENTED_EDGE('',*,*,#8211,.F.);
#10796=ORIENTED_EDGE('',*,*,#8221,.T.);
#10797=ORIENTED_EDGE('',*,*,#8218,.T.);
#10798=ORIENTED_EDGE('',*,*,#8215,.T.);
#10799=ORIENTED_EDGE('',*,*,#8212,.T.);
#10800=ORIENTED_EDGE('',*,*,#8209,.T.);
#10801=ORIENTED_EDGE('',*,*,#8206,.T.);
#10802=ORIENTED_EDGE('',*,*,#8203,.T.);
#10803=ORIENTED_EDGE('',*,*,#8200,.T.);
#10804=ORIENTED_EDGE('',*,*,#8197,.T.);
#10805=ORIENTED_EDGE('',*,*,#8194,.T.);
#10806=ORIENTED_EDGE('',*,*,#8191,.T.);
#10807=ORIENTED_EDGE('',*,*,#8188,.T.);
#10808=ORIENTED_EDGE('',*,*,#8220,.F.);
#10809=ORIENTED_EDGE('',*,*,#8210,.F.);
#10810=ORIENTED_EDGE('',*,*,#8214,.F.);
#10811=ORIENTED_EDGE('',*,*,#8217,.F.);
#10812=ORIENTED_EDGE('',*,*,#8207,.T.);
#10813=ORIENTED_EDGE('',*,*,#8204,.T.);
#10814=ORIENTED_EDGE('',*,*,#8201,.T.);
#10815=ORIENTED_EDGE('',*,*,#8198,.T.);
#10816=ORIENTED_EDGE('',*,*,#8195,.T.);
#10817=ORIENTED_EDGE('',*,*,#8192,.T.);
#10818=ORIENTED_EDGE('',*,*,#8189,.T.);
#10819=ORIENTED_EDGE('',*,*,#8186,.T.);
#10820=ORIENTED_EDGE('',*,*,#8222,.F.);
#10821=ORIENTED_EDGE('',*,*,#8223,.T.);
#10822=ORIENTED_EDGE('',*,*,#8224,.T.);
#10823=ORIENTED_EDGE('',*,*,#8223,.F.);
#10824=ORIENTED_EDGE('',*,*,#8224,.F.);
#10825=ORIENTED_EDGE('',*,*,#8225,.F.);
#10826=ORIENTED_EDGE('',*,*,#8226,.T.);
#10827=ORIENTED_EDGE('',*,*,#8227,.T.);
#10828=ORIENTED_EDGE('',*,*,#8226,.F.);
#10829=ORIENTED_EDGE('',*,*,#8227,.F.);
#10830=ORIENTED_EDGE('',*,*,#8228,.F.);
#10831=ORIENTED_EDGE('',*,*,#8229,.T.);
#10832=ORIENTED_EDGE('',*,*,#8230,.T.);
#10833=ORIENTED_EDGE('',*,*,#8229,.F.);
#10834=ORIENTED_EDGE('',*,*,#8230,.F.);
#10835=ORIENTED_EDGE('',*,*,#8231,.F.);
#10836=ORIENTED_EDGE('',*,*,#8232,.T.);
#10837=ORIENTED_EDGE('',*,*,#8233,.T.);
#10838=ORIENTED_EDGE('',*,*,#8232,.F.);
#10839=ORIENTED_EDGE('',*,*,#8233,.F.);
#10840=ORIENTED_EDGE('',*,*,#8234,.F.);
#10841=ORIENTED_EDGE('',*,*,#8235,.T.);
#10842=ORIENTED_EDGE('',*,*,#8236,.F.);
#10843=ORIENTED_EDGE('',*,*,#8237,.F.);
#10844=ORIENTED_EDGE('',*,*,#8238,.F.);
#10845=ORIENTED_EDGE('',*,*,#8237,.T.);
#10846=ORIENTED_EDGE('',*,*,#8239,.F.);
#10847=ORIENTED_EDGE('',*,*,#8240,.F.);
#10848=ORIENTED_EDGE('',*,*,#8222,.T.);
#10849=ORIENTED_EDGE('',*,*,#8225,.T.);
#10850=ORIENTED_EDGE('',*,*,#8228,.T.);
#10851=ORIENTED_EDGE('',*,*,#8231,.T.);
#10852=ORIENTED_EDGE('',*,*,#8241,.F.);
#10853=ORIENTED_EDGE('',*,*,#8240,.T.);
#10854=ORIENTED_EDGE('',*,*,#8242,.F.);
#10855=ORIENTED_EDGE('',*,*,#8243,.F.);
#10856=ORIENTED_EDGE('',*,*,#8244,.F.);
#10857=ORIENTED_EDGE('',*,*,#8243,.T.);
#10858=ORIENTED_EDGE('',*,*,#8245,.F.);
#10859=ORIENTED_EDGE('',*,*,#8246,.F.);
#10860=ORIENTED_EDGE('',*,*,#8247,.F.);
#10861=ORIENTED_EDGE('',*,*,#8246,.T.);
#10862=ORIENTED_EDGE('',*,*,#8248,.F.);
#10863=ORIENTED_EDGE('',*,*,#8249,.F.);
#10864=ORIENTED_EDGE('',*,*,#8250,.F.);
#10865=ORIENTED_EDGE('',*,*,#8249,.T.);
#10866=ORIENTED_EDGE('',*,*,#8251,.F.);
#10867=ORIENTED_EDGE('',*,*,#8252,.F.);
#10868=ORIENTED_EDGE('',*,*,#8253,.F.);
#10869=ORIENTED_EDGE('',*,*,#8252,.T.);
#10870=ORIENTED_EDGE('',*,*,#8254,.F.);
#10871=ORIENTED_EDGE('',*,*,#8255,.F.);
#10872=ORIENTED_EDGE('',*,*,#8256,.F.);
#10873=ORIENTED_EDGE('',*,*,#8255,.T.);
#10874=ORIENTED_EDGE('',*,*,#8257,.F.);
#10875=ORIENTED_EDGE('',*,*,#8258,.F.);
#10876=ORIENTED_EDGE('',*,*,#8259,.F.);
#10877=ORIENTED_EDGE('',*,*,#8258,.T.);
#10878=ORIENTED_EDGE('',*,*,#8260,.F.);
#10879=ORIENTED_EDGE('',*,*,#8261,.F.);
#10880=ORIENTED_EDGE('',*,*,#8262,.F.);
#10881=ORIENTED_EDGE('',*,*,#8261,.T.);
#10882=ORIENTED_EDGE('',*,*,#8263,.F.);
#10883=ORIENTED_EDGE('',*,*,#8264,.F.);
#10884=ORIENTED_EDGE('',*,*,#8265,.F.);
#10885=ORIENTED_EDGE('',*,*,#8264,.T.);
#10886=ORIENTED_EDGE('',*,*,#8266,.F.);
#10887=ORIENTED_EDGE('',*,*,#8267,.F.);
#10888=ORIENTED_EDGE('',*,*,#8268,.F.);
#10889=ORIENTED_EDGE('',*,*,#8267,.T.);
#10890=ORIENTED_EDGE('',*,*,#8269,.F.);
#10891=ORIENTED_EDGE('',*,*,#8270,.F.);
#10892=ORIENTED_EDGE('',*,*,#8271,.F.);
#10893=ORIENTED_EDGE('',*,*,#8270,.T.);
#10894=ORIENTED_EDGE('',*,*,#8272,.F.);
#10895=ORIENTED_EDGE('',*,*,#8273,.F.);
#10896=ORIENTED_EDGE('',*,*,#8274,.F.);
#10897=ORIENTED_EDGE('',*,*,#8273,.T.);
#10898=ORIENTED_EDGE('',*,*,#8275,.F.);
#10899=ORIENTED_EDGE('',*,*,#8276,.F.);
#10900=ORIENTED_EDGE('',*,*,#8277,.F.);
#10901=ORIENTED_EDGE('',*,*,#8276,.T.);
#10902=ORIENTED_EDGE('',*,*,#8278,.F.);
#10903=ORIENTED_EDGE('',*,*,#8279,.F.);
#10904=ORIENTED_EDGE('',*,*,#8280,.F.);
#10905=ORIENTED_EDGE('',*,*,#8279,.T.);
#10906=ORIENTED_EDGE('',*,*,#8281,.F.);
#10907=ORIENTED_EDGE('',*,*,#8282,.F.);
#10908=ORIENTED_EDGE('',*,*,#8283,.F.);
#10909=ORIENTED_EDGE('',*,*,#8282,.T.);
#10910=ORIENTED_EDGE('',*,*,#8284,.F.);
#10911=ORIENTED_EDGE('',*,*,#8285,.F.);
#10912=ORIENTED_EDGE('',*,*,#8286,.F.);
#10913=ORIENTED_EDGE('',*,*,#8285,.T.);
#10914=ORIENTED_EDGE('',*,*,#8287,.F.);
#10915=ORIENTED_EDGE('',*,*,#8288,.F.);
#10916=ORIENTED_EDGE('',*,*,#8289,.F.);
#10917=ORIENTED_EDGE('',*,*,#8288,.T.);
#10918=ORIENTED_EDGE('',*,*,#8290,.F.);
#10919=ORIENTED_EDGE('',*,*,#8291,.F.);
#10920=ORIENTED_EDGE('',*,*,#8292,.F.);
#10921=ORIENTED_EDGE('',*,*,#8291,.T.);
#10922=ORIENTED_EDGE('',*,*,#8293,.F.);
#10923=ORIENTED_EDGE('',*,*,#8294,.F.);
#10924=ORIENTED_EDGE('',*,*,#8295,.F.);
#10925=ORIENTED_EDGE('',*,*,#8294,.T.);
#10926=ORIENTED_EDGE('',*,*,#8296,.F.);
#10927=ORIENTED_EDGE('',*,*,#8297,.F.);
#10928=ORIENTED_EDGE('',*,*,#8298,.F.);
#10929=ORIENTED_EDGE('',*,*,#8297,.T.);
#10930=ORIENTED_EDGE('',*,*,#8299,.F.);
#10931=ORIENTED_EDGE('',*,*,#8300,.F.);
#10932=ORIENTED_EDGE('',*,*,#8301,.F.);
#10933=ORIENTED_EDGE('',*,*,#8300,.T.);
#10934=ORIENTED_EDGE('',*,*,#8302,.F.);
#10935=ORIENTED_EDGE('',*,*,#8303,.F.);
#10936=ORIENTED_EDGE('',*,*,#8304,.F.);
#10937=ORIENTED_EDGE('',*,*,#8303,.T.);
#10938=ORIENTED_EDGE('',*,*,#8305,.F.);
#10939=ORIENTED_EDGE('',*,*,#8306,.F.);
#10940=ORIENTED_EDGE('',*,*,#8307,.F.);
#10941=ORIENTED_EDGE('',*,*,#8306,.T.);
#10942=ORIENTED_EDGE('',*,*,#8308,.F.);
#10943=ORIENTED_EDGE('',*,*,#8309,.F.);
#10944=ORIENTED_EDGE('',*,*,#8310,.F.);
#10945=ORIENTED_EDGE('',*,*,#8309,.T.);
#10946=ORIENTED_EDGE('',*,*,#8311,.F.);
#10947=ORIENTED_EDGE('',*,*,#8312,.F.);
#10948=ORIENTED_EDGE('',*,*,#8313,.F.);
#10949=ORIENTED_EDGE('',*,*,#8312,.T.);
#10950=ORIENTED_EDGE('',*,*,#8314,.F.);
#10951=ORIENTED_EDGE('',*,*,#8315,.F.);
#10952=ORIENTED_EDGE('',*,*,#8316,.F.);
#10953=ORIENTED_EDGE('',*,*,#8315,.T.);
#10954=ORIENTED_EDGE('',*,*,#8317,.F.);
#10955=ORIENTED_EDGE('',*,*,#8318,.F.);
#10956=ORIENTED_EDGE('',*,*,#8319,.F.);
#10957=ORIENTED_EDGE('',*,*,#8318,.T.);
#10958=ORIENTED_EDGE('',*,*,#8320,.F.);
#10959=ORIENTED_EDGE('',*,*,#8321,.F.);
#10960=ORIENTED_EDGE('',*,*,#8322,.F.);
#10961=ORIENTED_EDGE('',*,*,#8321,.T.);
#10962=ORIENTED_EDGE('',*,*,#8323,.F.);
#10963=ORIENTED_EDGE('',*,*,#8324,.F.);
#10964=ORIENTED_EDGE('',*,*,#8325,.F.);
#10965=ORIENTED_EDGE('',*,*,#8324,.T.);
#10966=ORIENTED_EDGE('',*,*,#8326,.F.);
#10967=ORIENTED_EDGE('',*,*,#8327,.F.);
#10968=ORIENTED_EDGE('',*,*,#8328,.F.);
#10969=ORIENTED_EDGE('',*,*,#8327,.T.);
#10970=ORIENTED_EDGE('',*,*,#8329,.F.);
#10971=ORIENTED_EDGE('',*,*,#8330,.F.);
#10972=ORIENTED_EDGE('',*,*,#8331,.F.);
#10973=ORIENTED_EDGE('',*,*,#8330,.T.);
#10974=ORIENTED_EDGE('',*,*,#8332,.F.);
#10975=ORIENTED_EDGE('',*,*,#8333,.F.);
#10976=ORIENTED_EDGE('',*,*,#8334,.F.);
#10977=ORIENTED_EDGE('',*,*,#8333,.T.);
#10978=ORIENTED_EDGE('',*,*,#8335,.F.);
#10979=ORIENTED_EDGE('',*,*,#8336,.F.);
#10980=ORIENTED_EDGE('',*,*,#8337,.F.);
#10981=ORIENTED_EDGE('',*,*,#8336,.T.);
#10982=ORIENTED_EDGE('',*,*,#8338,.F.);
#10983=ORIENTED_EDGE('',*,*,#8339,.F.);
#10984=ORIENTED_EDGE('',*,*,#8340,.F.);
#10985=ORIENTED_EDGE('',*,*,#8339,.T.);
#10986=ORIENTED_EDGE('',*,*,#8341,.F.);
#10987=ORIENTED_EDGE('',*,*,#8342,.F.);
#10988=ORIENTED_EDGE('',*,*,#8343,.F.);
#10989=ORIENTED_EDGE('',*,*,#8342,.T.);
#10990=ORIENTED_EDGE('',*,*,#8344,.F.);
#10991=ORIENTED_EDGE('',*,*,#8345,.F.);
#10992=ORIENTED_EDGE('',*,*,#8346,.F.);
#10993=ORIENTED_EDGE('',*,*,#8345,.T.);
#10994=ORIENTED_EDGE('',*,*,#8347,.F.);
#10995=ORIENTED_EDGE('',*,*,#8348,.F.);
#10996=ORIENTED_EDGE('',*,*,#8349,.F.);
#10997=ORIENTED_EDGE('',*,*,#8348,.T.);
#10998=ORIENTED_EDGE('',*,*,#8350,.F.);
#10999=ORIENTED_EDGE('',*,*,#8351,.F.);
#11000=ORIENTED_EDGE('',*,*,#8352,.F.);
#11001=ORIENTED_EDGE('',*,*,#8351,.T.);
#11002=ORIENTED_EDGE('',*,*,#8353,.F.);
#11003=ORIENTED_EDGE('',*,*,#8354,.F.);
#11004=ORIENTED_EDGE('',*,*,#8355,.F.);
#11005=ORIENTED_EDGE('',*,*,#8354,.T.);
#11006=ORIENTED_EDGE('',*,*,#8356,.F.);
#11007=ORIENTED_EDGE('',*,*,#8357,.F.);
#11008=ORIENTED_EDGE('',*,*,#8358,.F.);
#11009=ORIENTED_EDGE('',*,*,#8357,.T.);
#11010=ORIENTED_EDGE('',*,*,#8359,.F.);
#11011=ORIENTED_EDGE('',*,*,#8360,.F.);
#11012=ORIENTED_EDGE('',*,*,#8361,.F.);
#11013=ORIENTED_EDGE('',*,*,#8360,.T.);
#11014=ORIENTED_EDGE('',*,*,#8362,.F.);
#11015=ORIENTED_EDGE('',*,*,#8363,.F.);
#11016=ORIENTED_EDGE('',*,*,#8364,.F.);
#11017=ORIENTED_EDGE('',*,*,#8363,.T.);
#11018=ORIENTED_EDGE('',*,*,#8365,.F.);
#11019=ORIENTED_EDGE('',*,*,#8366,.F.);
#11020=ORIENTED_EDGE('',*,*,#8367,.F.);
#11021=ORIENTED_EDGE('',*,*,#8366,.T.);
#11022=ORIENTED_EDGE('',*,*,#8368,.F.);
#11023=ORIENTED_EDGE('',*,*,#8369,.F.);
#11024=ORIENTED_EDGE('',*,*,#8370,.F.);
#11025=ORIENTED_EDGE('',*,*,#8369,.T.);
#11026=ORIENTED_EDGE('',*,*,#8371,.F.);
#11027=ORIENTED_EDGE('',*,*,#8372,.F.);
#11028=ORIENTED_EDGE('',*,*,#8373,.F.);
#11029=ORIENTED_EDGE('',*,*,#8372,.T.);
#11030=ORIENTED_EDGE('',*,*,#8374,.F.);
#11031=ORIENTED_EDGE('',*,*,#8375,.F.);
#11032=ORIENTED_EDGE('',*,*,#8376,.F.);
#11033=ORIENTED_EDGE('',*,*,#8375,.T.);
#11034=ORIENTED_EDGE('',*,*,#8377,.F.);
#11035=ORIENTED_EDGE('',*,*,#8378,.F.);
#11036=ORIENTED_EDGE('',*,*,#8379,.F.);
#11037=ORIENTED_EDGE('',*,*,#8378,.T.);
#11038=ORIENTED_EDGE('',*,*,#8380,.F.);
#11039=ORIENTED_EDGE('',*,*,#8381,.F.);
#11040=ORIENTED_EDGE('',*,*,#8382,.F.);
#11041=ORIENTED_EDGE('',*,*,#8381,.T.);
#11042=ORIENTED_EDGE('',*,*,#8383,.F.);
#11043=ORIENTED_EDGE('',*,*,#8384,.F.);
#11044=ORIENTED_EDGE('',*,*,#8385,.F.);
#11045=ORIENTED_EDGE('',*,*,#8384,.T.);
#11046=ORIENTED_EDGE('',*,*,#8386,.F.);
#11047=ORIENTED_EDGE('',*,*,#8387,.F.);
#11048=ORIENTED_EDGE('',*,*,#8388,.F.);
#11049=ORIENTED_EDGE('',*,*,#8387,.T.);
#11050=ORIENTED_EDGE('',*,*,#8389,.F.);
#11051=ORIENTED_EDGE('',*,*,#8390,.F.);
#11052=ORIENTED_EDGE('',*,*,#8391,.F.);
#11053=ORIENTED_EDGE('',*,*,#8390,.T.);
#11054=ORIENTED_EDGE('',*,*,#8392,.F.);
#11055=ORIENTED_EDGE('',*,*,#8393,.F.);
#11056=ORIENTED_EDGE('',*,*,#8394,.F.);
#11057=ORIENTED_EDGE('',*,*,#8393,.T.);
#11058=ORIENTED_EDGE('',*,*,#8395,.F.);
#11059=ORIENTED_EDGE('',*,*,#8396,.F.);
#11060=ORIENTED_EDGE('',*,*,#8397,.F.);
#11061=ORIENTED_EDGE('',*,*,#8396,.T.);
#11062=ORIENTED_EDGE('',*,*,#8398,.F.);
#11063=ORIENTED_EDGE('',*,*,#8399,.F.);
#11064=ORIENTED_EDGE('',*,*,#8400,.F.);
#11065=ORIENTED_EDGE('',*,*,#8399,.T.);
#11066=ORIENTED_EDGE('',*,*,#8401,.F.);
#11067=ORIENTED_EDGE('',*,*,#8402,.F.);
#11068=ORIENTED_EDGE('',*,*,#8403,.F.);
#11069=ORIENTED_EDGE('',*,*,#8402,.T.);
#11070=ORIENTED_EDGE('',*,*,#8404,.F.);
#11071=ORIENTED_EDGE('',*,*,#8405,.F.);
#11072=ORIENTED_EDGE('',*,*,#8406,.F.);
#11073=ORIENTED_EDGE('',*,*,#8405,.T.);
#11074=ORIENTED_EDGE('',*,*,#8407,.F.);
#11075=ORIENTED_EDGE('',*,*,#8408,.F.);
#11076=ORIENTED_EDGE('',*,*,#8409,.F.);
#11077=ORIENTED_EDGE('',*,*,#8408,.T.);
#11078=ORIENTED_EDGE('',*,*,#8410,.F.);
#11079=ORIENTED_EDGE('',*,*,#8411,.F.);
#11080=ORIENTED_EDGE('',*,*,#8412,.F.);
#11081=ORIENTED_EDGE('',*,*,#8411,.T.);
#11082=ORIENTED_EDGE('',*,*,#8413,.F.);
#11083=ORIENTED_EDGE('',*,*,#8414,.F.);
#11084=ORIENTED_EDGE('',*,*,#8415,.F.);
#11085=ORIENTED_EDGE('',*,*,#8414,.T.);
#11086=ORIENTED_EDGE('',*,*,#8416,.F.);
#11087=ORIENTED_EDGE('',*,*,#8417,.F.);
#11088=ORIENTED_EDGE('',*,*,#8418,.F.);
#11089=ORIENTED_EDGE('',*,*,#8417,.T.);
#11090=ORIENTED_EDGE('',*,*,#8419,.F.);
#11091=ORIENTED_EDGE('',*,*,#8420,.F.);
#11092=ORIENTED_EDGE('',*,*,#8421,.F.);
#11093=ORIENTED_EDGE('',*,*,#8420,.T.);
#11094=ORIENTED_EDGE('',*,*,#8422,.F.);
#11095=ORIENTED_EDGE('',*,*,#8423,.F.);
#11096=ORIENTED_EDGE('',*,*,#8424,.F.);
#11097=ORIENTED_EDGE('',*,*,#8423,.T.);
#11098=ORIENTED_EDGE('',*,*,#8425,.F.);
#11099=ORIENTED_EDGE('',*,*,#8426,.F.);
#11100=ORIENTED_EDGE('',*,*,#8427,.F.);
#11101=ORIENTED_EDGE('',*,*,#8426,.T.);
#11102=ORIENTED_EDGE('',*,*,#8428,.F.);
#11103=ORIENTED_EDGE('',*,*,#8429,.F.);
#11104=ORIENTED_EDGE('',*,*,#8430,.F.);
#11105=ORIENTED_EDGE('',*,*,#8429,.T.);
#11106=ORIENTED_EDGE('',*,*,#8431,.F.);
#11107=ORIENTED_EDGE('',*,*,#8432,.F.);
#11108=ORIENTED_EDGE('',*,*,#8433,.F.);
#11109=ORIENTED_EDGE('',*,*,#8432,.T.);
#11110=ORIENTED_EDGE('',*,*,#8434,.F.);
#11111=ORIENTED_EDGE('',*,*,#8435,.F.);
#11112=ORIENTED_EDGE('',*,*,#8436,.F.);
#11113=ORIENTED_EDGE('',*,*,#8435,.T.);
#11114=ORIENTED_EDGE('',*,*,#8437,.F.);
#11115=ORIENTED_EDGE('',*,*,#8438,.F.);
#11116=ORIENTED_EDGE('',*,*,#8439,.F.);
#11117=ORIENTED_EDGE('',*,*,#8438,.T.);
#11118=ORIENTED_EDGE('',*,*,#8440,.F.);
#11119=ORIENTED_EDGE('',*,*,#8441,.F.);
#11120=ORIENTED_EDGE('',*,*,#8442,.F.);
#11121=ORIENTED_EDGE('',*,*,#8441,.T.);
#11122=ORIENTED_EDGE('',*,*,#8443,.F.);
#11123=ORIENTED_EDGE('',*,*,#8444,.F.);
#11124=ORIENTED_EDGE('',*,*,#8445,.F.);
#11125=ORIENTED_EDGE('',*,*,#8444,.T.);
#11126=ORIENTED_EDGE('',*,*,#8446,.F.);
#11127=ORIENTED_EDGE('',*,*,#8447,.F.);
#11128=ORIENTED_EDGE('',*,*,#8448,.F.);
#11129=ORIENTED_EDGE('',*,*,#8447,.T.);
#11130=ORIENTED_EDGE('',*,*,#8449,.F.);
#11131=ORIENTED_EDGE('',*,*,#8450,.F.);
#11132=ORIENTED_EDGE('',*,*,#8451,.F.);
#11133=ORIENTED_EDGE('',*,*,#8450,.T.);
#11134=ORIENTED_EDGE('',*,*,#8452,.F.);
#11135=ORIENTED_EDGE('',*,*,#8453,.F.);
#11136=ORIENTED_EDGE('',*,*,#8454,.F.);
#11137=ORIENTED_EDGE('',*,*,#8453,.T.);
#11138=ORIENTED_EDGE('',*,*,#8455,.F.);
#11139=ORIENTED_EDGE('',*,*,#8456,.F.);
#11140=ORIENTED_EDGE('',*,*,#8457,.F.);
#11141=ORIENTED_EDGE('',*,*,#8456,.T.);
#11142=ORIENTED_EDGE('',*,*,#8458,.F.);
#11143=ORIENTED_EDGE('',*,*,#8459,.F.);
#11144=ORIENTED_EDGE('',*,*,#8460,.F.);
#11145=ORIENTED_EDGE('',*,*,#8459,.T.);
#11146=ORIENTED_EDGE('',*,*,#8461,.F.);
#11147=ORIENTED_EDGE('',*,*,#8462,.F.);
#11148=ORIENTED_EDGE('',*,*,#8463,.F.);
#11149=ORIENTED_EDGE('',*,*,#8462,.T.);
#11150=ORIENTED_EDGE('',*,*,#8464,.F.);
#11151=ORIENTED_EDGE('',*,*,#8465,.F.);
#11152=ORIENTED_EDGE('',*,*,#8466,.F.);
#11153=ORIENTED_EDGE('',*,*,#8465,.T.);
#11154=ORIENTED_EDGE('',*,*,#8467,.F.);
#11155=ORIENTED_EDGE('',*,*,#8468,.F.);
#11156=ORIENTED_EDGE('',*,*,#8469,.F.);
#11157=ORIENTED_EDGE('',*,*,#8468,.T.);
#11158=ORIENTED_EDGE('',*,*,#8470,.F.);
#11159=ORIENTED_EDGE('',*,*,#8471,.F.);
#11160=ORIENTED_EDGE('',*,*,#8472,.F.);
#11161=ORIENTED_EDGE('',*,*,#8471,.T.);
#11162=ORIENTED_EDGE('',*,*,#8473,.F.);
#11163=ORIENTED_EDGE('',*,*,#8474,.F.);
#11164=ORIENTED_EDGE('',*,*,#8475,.F.);
#11165=ORIENTED_EDGE('',*,*,#8474,.T.);
#11166=ORIENTED_EDGE('',*,*,#8476,.F.);
#11167=ORIENTED_EDGE('',*,*,#8477,.F.);
#11168=ORIENTED_EDGE('',*,*,#8478,.F.);
#11169=ORIENTED_EDGE('',*,*,#8477,.T.);
#11170=ORIENTED_EDGE('',*,*,#8479,.F.);
#11171=ORIENTED_EDGE('',*,*,#8480,.F.);
#11172=ORIENTED_EDGE('',*,*,#8481,.F.);
#11173=ORIENTED_EDGE('',*,*,#8480,.T.);
#11174=ORIENTED_EDGE('',*,*,#8482,.F.);
#11175=ORIENTED_EDGE('',*,*,#8483,.F.);
#11176=ORIENTED_EDGE('',*,*,#8484,.F.);
#11177=ORIENTED_EDGE('',*,*,#8483,.T.);
#11178=ORIENTED_EDGE('',*,*,#8485,.F.);
#11179=ORIENTED_EDGE('',*,*,#8486,.F.);
#11180=ORIENTED_EDGE('',*,*,#8487,.F.);
#11181=ORIENTED_EDGE('',*,*,#8486,.T.);
#11182=ORIENTED_EDGE('',*,*,#8488,.F.);
#11183=ORIENTED_EDGE('',*,*,#8489,.F.);
#11184=ORIENTED_EDGE('',*,*,#8490,.F.);
#11185=ORIENTED_EDGE('',*,*,#8489,.T.);
#11186=ORIENTED_EDGE('',*,*,#8491,.F.);
#11187=ORIENTED_EDGE('',*,*,#8492,.F.);
#11188=ORIENTED_EDGE('',*,*,#8493,.F.);
#11189=ORIENTED_EDGE('',*,*,#8492,.T.);
#11190=ORIENTED_EDGE('',*,*,#8494,.F.);
#11191=ORIENTED_EDGE('',*,*,#8495,.F.);
#11192=ORIENTED_EDGE('',*,*,#8496,.F.);
#11193=ORIENTED_EDGE('',*,*,#8495,.T.);
#11194=ORIENTED_EDGE('',*,*,#8497,.F.);
#11195=ORIENTED_EDGE('',*,*,#8498,.F.);
#11196=ORIENTED_EDGE('',*,*,#8499,.F.);
#11197=ORIENTED_EDGE('',*,*,#8498,.T.);
#11198=ORIENTED_EDGE('',*,*,#8500,.F.);
#11199=ORIENTED_EDGE('',*,*,#8501,.F.);
#11200=ORIENTED_EDGE('',*,*,#8502,.F.);
#11201=ORIENTED_EDGE('',*,*,#8501,.T.);
#11202=ORIENTED_EDGE('',*,*,#8503,.F.);
#11203=ORIENTED_EDGE('',*,*,#8504,.F.);
#11204=ORIENTED_EDGE('',*,*,#8505,.F.);
#11205=ORIENTED_EDGE('',*,*,#8504,.T.);
#11206=ORIENTED_EDGE('',*,*,#8506,.F.);
#11207=ORIENTED_EDGE('',*,*,#8507,.F.);
#11208=ORIENTED_EDGE('',*,*,#8508,.F.);
#11209=ORIENTED_EDGE('',*,*,#8507,.T.);
#11210=ORIENTED_EDGE('',*,*,#8509,.F.);
#11211=ORIENTED_EDGE('',*,*,#8510,.F.);
#11212=ORIENTED_EDGE('',*,*,#8511,.F.);
#11213=ORIENTED_EDGE('',*,*,#8510,.T.);
#11214=ORIENTED_EDGE('',*,*,#8512,.F.);
#11215=ORIENTED_EDGE('',*,*,#8513,.F.);
#11216=ORIENTED_EDGE('',*,*,#8514,.F.);
#11217=ORIENTED_EDGE('',*,*,#8513,.T.);
#11218=ORIENTED_EDGE('',*,*,#8515,.F.);
#11219=ORIENTED_EDGE('',*,*,#8516,.F.);
#11220=ORIENTED_EDGE('',*,*,#8517,.F.);
#11221=ORIENTED_EDGE('',*,*,#8516,.T.);
#11222=ORIENTED_EDGE('',*,*,#8518,.F.);
#11223=ORIENTED_EDGE('',*,*,#8519,.F.);
#11224=ORIENTED_EDGE('',*,*,#8520,.F.);
#11225=ORIENTED_EDGE('',*,*,#8519,.T.);
#11226=ORIENTED_EDGE('',*,*,#8521,.F.);
#11227=ORIENTED_EDGE('',*,*,#8522,.F.);
#11228=ORIENTED_EDGE('',*,*,#8523,.F.);
#11229=ORIENTED_EDGE('',*,*,#8522,.T.);
#11230=ORIENTED_EDGE('',*,*,#8524,.F.);
#11231=ORIENTED_EDGE('',*,*,#8525,.F.);
#11232=ORIENTED_EDGE('',*,*,#8526,.F.);
#11233=ORIENTED_EDGE('',*,*,#8525,.T.);
#11234=ORIENTED_EDGE('',*,*,#8527,.F.);
#11235=ORIENTED_EDGE('',*,*,#8528,.F.);
#11236=ORIENTED_EDGE('',*,*,#8529,.F.);
#11237=ORIENTED_EDGE('',*,*,#8528,.T.);
#11238=ORIENTED_EDGE('',*,*,#8530,.F.);
#11239=ORIENTED_EDGE('',*,*,#8531,.F.);
#11240=ORIENTED_EDGE('',*,*,#8532,.F.);
#11241=ORIENTED_EDGE('',*,*,#8531,.T.);
#11242=ORIENTED_EDGE('',*,*,#8533,.F.);
#11243=ORIENTED_EDGE('',*,*,#8534,.F.);
#11244=ORIENTED_EDGE('',*,*,#8535,.F.);
#11245=ORIENTED_EDGE('',*,*,#8534,.T.);
#11246=ORIENTED_EDGE('',*,*,#8536,.F.);
#11247=ORIENTED_EDGE('',*,*,#8537,.F.);
#11248=ORIENTED_EDGE('',*,*,#8538,.F.);
#11249=ORIENTED_EDGE('',*,*,#8537,.T.);
#11250=ORIENTED_EDGE('',*,*,#8539,.F.);
#11251=ORIENTED_EDGE('',*,*,#8540,.F.);
#11252=ORIENTED_EDGE('',*,*,#8541,.F.);
#11253=ORIENTED_EDGE('',*,*,#8540,.T.);
#11254=ORIENTED_EDGE('',*,*,#8542,.F.);
#11255=ORIENTED_EDGE('',*,*,#8543,.F.);
#11256=ORIENTED_EDGE('',*,*,#8544,.F.);
#11257=ORIENTED_EDGE('',*,*,#8543,.T.);
#11258=ORIENTED_EDGE('',*,*,#8545,.F.);
#11259=ORIENTED_EDGE('',*,*,#8546,.F.);
#11260=ORIENTED_EDGE('',*,*,#8547,.F.);
#11261=ORIENTED_EDGE('',*,*,#8546,.T.);
#11262=ORIENTED_EDGE('',*,*,#8548,.F.);
#11263=ORIENTED_EDGE('',*,*,#8549,.F.);
#11264=ORIENTED_EDGE('',*,*,#8550,.F.);
#11265=ORIENTED_EDGE('',*,*,#8549,.T.);
#11266=ORIENTED_EDGE('',*,*,#8551,.F.);
#11267=ORIENTED_EDGE('',*,*,#8552,.F.);
#11268=ORIENTED_EDGE('',*,*,#8553,.F.);
#11269=ORIENTED_EDGE('',*,*,#8552,.T.);
#11270=ORIENTED_EDGE('',*,*,#8554,.F.);
#11271=ORIENTED_EDGE('',*,*,#8555,.F.);
#11272=ORIENTED_EDGE('',*,*,#8556,.F.);
#11273=ORIENTED_EDGE('',*,*,#8555,.T.);
#11274=ORIENTED_EDGE('',*,*,#8557,.F.);
#11275=ORIENTED_EDGE('',*,*,#8558,.F.);
#11276=ORIENTED_EDGE('',*,*,#8559,.F.);
#11277=ORIENTED_EDGE('',*,*,#8558,.T.);
#11278=ORIENTED_EDGE('',*,*,#8560,.F.);
#11279=ORIENTED_EDGE('',*,*,#8561,.F.);
#11280=ORIENTED_EDGE('',*,*,#8562,.F.);
#11281=ORIENTED_EDGE('',*,*,#8561,.T.);
#11282=ORIENTED_EDGE('',*,*,#8563,.F.);
#11283=ORIENTED_EDGE('',*,*,#8564,.F.);
#11284=ORIENTED_EDGE('',*,*,#8565,.F.);
#11285=ORIENTED_EDGE('',*,*,#8564,.T.);
#11286=ORIENTED_EDGE('',*,*,#8566,.F.);
#11287=ORIENTED_EDGE('',*,*,#8567,.F.);
#11288=ORIENTED_EDGE('',*,*,#8568,.F.);
#11289=ORIENTED_EDGE('',*,*,#8567,.T.);
#11290=ORIENTED_EDGE('',*,*,#8569,.F.);
#11291=ORIENTED_EDGE('',*,*,#8570,.F.);
#11292=ORIENTED_EDGE('',*,*,#8571,.F.);
#11293=ORIENTED_EDGE('',*,*,#8570,.T.);
#11294=ORIENTED_EDGE('',*,*,#8572,.F.);
#11295=ORIENTED_EDGE('',*,*,#8573,.F.);
#11296=ORIENTED_EDGE('',*,*,#8574,.F.);
#11297=ORIENTED_EDGE('',*,*,#8573,.T.);
#11298=ORIENTED_EDGE('',*,*,#8575,.F.);
#11299=ORIENTED_EDGE('',*,*,#8576,.F.);
#11300=ORIENTED_EDGE('',*,*,#8577,.F.);
#11301=ORIENTED_EDGE('',*,*,#8576,.T.);
#11302=ORIENTED_EDGE('',*,*,#8578,.F.);
#11303=ORIENTED_EDGE('',*,*,#8579,.F.);
#11304=ORIENTED_EDGE('',*,*,#8580,.F.);
#11305=ORIENTED_EDGE('',*,*,#8579,.T.);
#11306=ORIENTED_EDGE('',*,*,#8581,.F.);
#11307=ORIENTED_EDGE('',*,*,#8582,.F.);
#11308=ORIENTED_EDGE('',*,*,#8583,.F.);
#11309=ORIENTED_EDGE('',*,*,#8582,.T.);
#11310=ORIENTED_EDGE('',*,*,#8584,.F.);
#11311=ORIENTED_EDGE('',*,*,#8585,.F.);
#11312=ORIENTED_EDGE('',*,*,#8586,.F.);
#11313=ORIENTED_EDGE('',*,*,#8585,.T.);
#11314=ORIENTED_EDGE('',*,*,#8587,.F.);
#11315=ORIENTED_EDGE('',*,*,#8588,.F.);
#11316=ORIENTED_EDGE('',*,*,#8589,.F.);
#11317=ORIENTED_EDGE('',*,*,#8588,.T.);
#11318=ORIENTED_EDGE('',*,*,#8590,.F.);
#11319=ORIENTED_EDGE('',*,*,#8591,.F.);
#11320=ORIENTED_EDGE('',*,*,#8592,.F.);
#11321=ORIENTED_EDGE('',*,*,#8591,.T.);
#11322=ORIENTED_EDGE('',*,*,#8593,.F.);
#11323=ORIENTED_EDGE('',*,*,#8594,.F.);
#11324=ORIENTED_EDGE('',*,*,#8595,.F.);
#11325=ORIENTED_EDGE('',*,*,#8594,.T.);
#11326=ORIENTED_EDGE('',*,*,#8596,.F.);
#11327=ORIENTED_EDGE('',*,*,#8597,.F.);
#11328=ORIENTED_EDGE('',*,*,#8598,.F.);
#11329=ORIENTED_EDGE('',*,*,#8597,.T.);
#11330=ORIENTED_EDGE('',*,*,#8599,.F.);
#11331=ORIENTED_EDGE('',*,*,#8600,.F.);
#11332=ORIENTED_EDGE('',*,*,#8601,.F.);
#11333=ORIENTED_EDGE('',*,*,#8600,.T.);
#11334=ORIENTED_EDGE('',*,*,#8602,.F.);
#11335=ORIENTED_EDGE('',*,*,#8603,.F.);
#11336=ORIENTED_EDGE('',*,*,#8604,.F.);
#11337=ORIENTED_EDGE('',*,*,#8603,.T.);
#11338=ORIENTED_EDGE('',*,*,#8605,.F.);
#11339=ORIENTED_EDGE('',*,*,#8606,.F.);
#11340=ORIENTED_EDGE('',*,*,#8607,.F.);
#11341=ORIENTED_EDGE('',*,*,#8606,.T.);
#11342=ORIENTED_EDGE('',*,*,#8608,.F.);
#11343=ORIENTED_EDGE('',*,*,#8609,.F.);
#11344=ORIENTED_EDGE('',*,*,#8610,.F.);
#11345=ORIENTED_EDGE('',*,*,#8609,.T.);
#11346=ORIENTED_EDGE('',*,*,#8611,.F.);
#11347=ORIENTED_EDGE('',*,*,#8612,.F.);
#11348=ORIENTED_EDGE('',*,*,#8613,.F.);
#11349=ORIENTED_EDGE('',*,*,#8612,.T.);
#11350=ORIENTED_EDGE('',*,*,#8614,.F.);
#11351=ORIENTED_EDGE('',*,*,#8615,.F.);
#11352=ORIENTED_EDGE('',*,*,#8616,.F.);
#11353=ORIENTED_EDGE('',*,*,#8615,.T.);
#11354=ORIENTED_EDGE('',*,*,#8617,.F.);
#11355=ORIENTED_EDGE('',*,*,#8235,.F.);
#11356=ORIENTED_EDGE('',*,*,#8617,.T.);
#11357=ORIENTED_EDGE('',*,*,#8614,.T.);
#11358=ORIENTED_EDGE('',*,*,#8611,.T.);
#11359=ORIENTED_EDGE('',*,*,#8608,.T.);
#11360=ORIENTED_EDGE('',*,*,#8605,.T.);
#11361=ORIENTED_EDGE('',*,*,#8602,.T.);
#11362=ORIENTED_EDGE('',*,*,#8599,.T.);
#11363=ORIENTED_EDGE('',*,*,#8596,.T.);
#11364=ORIENTED_EDGE('',*,*,#8593,.T.);
#11365=ORIENTED_EDGE('',*,*,#8590,.T.);
#11366=ORIENTED_EDGE('',*,*,#8587,.T.);
#11367=ORIENTED_EDGE('',*,*,#8584,.T.);
#11368=ORIENTED_EDGE('',*,*,#8581,.T.);
#11369=ORIENTED_EDGE('',*,*,#8578,.T.);
#11370=ORIENTED_EDGE('',*,*,#8575,.T.);
#11371=ORIENTED_EDGE('',*,*,#8572,.T.);
#11372=ORIENTED_EDGE('',*,*,#8569,.T.);
#11373=ORIENTED_EDGE('',*,*,#8566,.T.);
#11374=ORIENTED_EDGE('',*,*,#8563,.T.);
#11375=ORIENTED_EDGE('',*,*,#8560,.T.);
#11376=ORIENTED_EDGE('',*,*,#8557,.T.);
#11377=ORIENTED_EDGE('',*,*,#8554,.T.);
#11378=ORIENTED_EDGE('',*,*,#8551,.T.);
#11379=ORIENTED_EDGE('',*,*,#8548,.T.);
#11380=ORIENTED_EDGE('',*,*,#8545,.T.);
#11381=ORIENTED_EDGE('',*,*,#8542,.T.);
#11382=ORIENTED_EDGE('',*,*,#8539,.T.);
#11383=ORIENTED_EDGE('',*,*,#8536,.T.);
#11384=ORIENTED_EDGE('',*,*,#8533,.T.);
#11385=ORIENTED_EDGE('',*,*,#8530,.T.);
#11386=ORIENTED_EDGE('',*,*,#8527,.T.);
#11387=ORIENTED_EDGE('',*,*,#8524,.T.);
#11388=ORIENTED_EDGE('',*,*,#8521,.T.);
#11389=ORIENTED_EDGE('',*,*,#8518,.T.);
#11390=ORIENTED_EDGE('',*,*,#8515,.T.);
#11391=ORIENTED_EDGE('',*,*,#8512,.T.);
#11392=ORIENTED_EDGE('',*,*,#8509,.T.);
#11393=ORIENTED_EDGE('',*,*,#8506,.T.);
#11394=ORIENTED_EDGE('',*,*,#8503,.T.);
#11395=ORIENTED_EDGE('',*,*,#8500,.T.);
#11396=ORIENTED_EDGE('',*,*,#8497,.T.);
#11397=ORIENTED_EDGE('',*,*,#8494,.T.);
#11398=ORIENTED_EDGE('',*,*,#8491,.T.);
#11399=ORIENTED_EDGE('',*,*,#8488,.T.);
#11400=ORIENTED_EDGE('',*,*,#8485,.T.);
#11401=ORIENTED_EDGE('',*,*,#8482,.T.);
#11402=ORIENTED_EDGE('',*,*,#8479,.T.);
#11403=ORIENTED_EDGE('',*,*,#8476,.T.);
#11404=ORIENTED_EDGE('',*,*,#8473,.T.);
#11405=ORIENTED_EDGE('',*,*,#8470,.T.);
#11406=ORIENTED_EDGE('',*,*,#8467,.T.);
#11407=ORIENTED_EDGE('',*,*,#8464,.T.);
#11408=ORIENTED_EDGE('',*,*,#8461,.T.);
#11409=ORIENTED_EDGE('',*,*,#8458,.T.);
#11410=ORIENTED_EDGE('',*,*,#8455,.T.);
#11411=ORIENTED_EDGE('',*,*,#8452,.T.);
#11412=ORIENTED_EDGE('',*,*,#8449,.T.);
#11413=ORIENTED_EDGE('',*,*,#8446,.T.);
#11414=ORIENTED_EDGE('',*,*,#8443,.T.);
#11415=ORIENTED_EDGE('',*,*,#8440,.T.);
#11416=ORIENTED_EDGE('',*,*,#8437,.T.);
#11417=ORIENTED_EDGE('',*,*,#8434,.T.);
#11418=ORIENTED_EDGE('',*,*,#8431,.T.);
#11419=ORIENTED_EDGE('',*,*,#8428,.T.);
#11420=ORIENTED_EDGE('',*,*,#8425,.T.);
#11421=ORIENTED_EDGE('',*,*,#8422,.T.);
#11422=ORIENTED_EDGE('',*,*,#8419,.T.);
#11423=ORIENTED_EDGE('',*,*,#8416,.T.);
#11424=ORIENTED_EDGE('',*,*,#8413,.T.);
#11425=ORIENTED_EDGE('',*,*,#8410,.T.);
#11426=ORIENTED_EDGE('',*,*,#8407,.T.);
#11427=ORIENTED_EDGE('',*,*,#8404,.T.);
#11428=ORIENTED_EDGE('',*,*,#8401,.T.);
#11429=ORIENTED_EDGE('',*,*,#8398,.T.);
#11430=ORIENTED_EDGE('',*,*,#8395,.T.);
#11431=ORIENTED_EDGE('',*,*,#8392,.T.);
#11432=ORIENTED_EDGE('',*,*,#8389,.T.);
#11433=ORIENTED_EDGE('',*,*,#8386,.T.);
#11434=ORIENTED_EDGE('',*,*,#8383,.T.);
#11435=ORIENTED_EDGE('',*,*,#8380,.T.);
#11436=ORIENTED_EDGE('',*,*,#8377,.T.);
#11437=ORIENTED_EDGE('',*,*,#8374,.T.);
#11438=ORIENTED_EDGE('',*,*,#8371,.T.);
#11439=ORIENTED_EDGE('',*,*,#8368,.T.);
#11440=ORIENTED_EDGE('',*,*,#8365,.T.);
#11441=ORIENTED_EDGE('',*,*,#8362,.T.);
#11442=ORIENTED_EDGE('',*,*,#8359,.T.);
#11443=ORIENTED_EDGE('',*,*,#8356,.T.);
#11444=ORIENTED_EDGE('',*,*,#8353,.T.);
#11445=ORIENTED_EDGE('',*,*,#8350,.T.);
#11446=ORIENTED_EDGE('',*,*,#8347,.T.);
#11447=ORIENTED_EDGE('',*,*,#8344,.T.);
#11448=ORIENTED_EDGE('',*,*,#8341,.T.);
#11449=ORIENTED_EDGE('',*,*,#8338,.T.);
#11450=ORIENTED_EDGE('',*,*,#8335,.T.);
#11451=ORIENTED_EDGE('',*,*,#8332,.T.);
#11452=ORIENTED_EDGE('',*,*,#8329,.T.);
#11453=ORIENTED_EDGE('',*,*,#8326,.T.);
#11454=ORIENTED_EDGE('',*,*,#8323,.T.);
#11455=ORIENTED_EDGE('',*,*,#8320,.T.);
#11456=ORIENTED_EDGE('',*,*,#8317,.T.);
#11457=ORIENTED_EDGE('',*,*,#8314,.T.);
#11458=ORIENTED_EDGE('',*,*,#8311,.T.);
#11459=ORIENTED_EDGE('',*,*,#8308,.T.);
#11460=ORIENTED_EDGE('',*,*,#8305,.T.);
#11461=ORIENTED_EDGE('',*,*,#8302,.T.);
#11462=ORIENTED_EDGE('',*,*,#8299,.T.);
#11463=ORIENTED_EDGE('',*,*,#8296,.T.);
#11464=ORIENTED_EDGE('',*,*,#8293,.T.);
#11465=ORIENTED_EDGE('',*,*,#8290,.T.);
#11466=ORIENTED_EDGE('',*,*,#8287,.T.);
#11467=ORIENTED_EDGE('',*,*,#8284,.T.);
#11468=ORIENTED_EDGE('',*,*,#8281,.T.);
#11469=ORIENTED_EDGE('',*,*,#8278,.T.);
#11470=ORIENTED_EDGE('',*,*,#8275,.T.);
#11471=ORIENTED_EDGE('',*,*,#8272,.T.);
#11472=ORIENTED_EDGE('',*,*,#8269,.T.);
#11473=ORIENTED_EDGE('',*,*,#8266,.T.);
#11474=ORIENTED_EDGE('',*,*,#8263,.T.);
#11475=ORIENTED_EDGE('',*,*,#8260,.T.);
#11476=ORIENTED_EDGE('',*,*,#8257,.T.);
#11477=ORIENTED_EDGE('',*,*,#8254,.T.);
#11478=ORIENTED_EDGE('',*,*,#8251,.T.);
#11479=ORIENTED_EDGE('',*,*,#8248,.T.);
#11480=ORIENTED_EDGE('',*,*,#8245,.T.);
#11481=ORIENTED_EDGE('',*,*,#8242,.T.);
#11482=ORIENTED_EDGE('',*,*,#8239,.T.);
#11483=ORIENTED_EDGE('',*,*,#8236,.T.);
#11484=ORIENTED_EDGE('',*,*,#8616,.T.);
#11485=ORIENTED_EDGE('',*,*,#8234,.T.);
#11486=ORIENTED_EDGE('',*,*,#8238,.T.);
#11487=ORIENTED_EDGE('',*,*,#8241,.T.);
#11488=ORIENTED_EDGE('',*,*,#8244,.T.);
#11489=ORIENTED_EDGE('',*,*,#8247,.T.);
#11490=ORIENTED_EDGE('',*,*,#8250,.T.);
#11491=ORIENTED_EDGE('',*,*,#8253,.T.);
#11492=ORIENTED_EDGE('',*,*,#8256,.T.);
#11493=ORIENTED_EDGE('',*,*,#8259,.T.);
#11494=ORIENTED_EDGE('',*,*,#8262,.T.);
#11495=ORIENTED_EDGE('',*,*,#8265,.T.);
#11496=ORIENTED_EDGE('',*,*,#8268,.T.);
#11497=ORIENTED_EDGE('',*,*,#8271,.T.);
#11498=ORIENTED_EDGE('',*,*,#8274,.T.);
#11499=ORIENTED_EDGE('',*,*,#8277,.T.);
#11500=ORIENTED_EDGE('',*,*,#8280,.T.);
#11501=ORIENTED_EDGE('',*,*,#8283,.T.);
#11502=ORIENTED_EDGE('',*,*,#8286,.T.);
#11503=ORIENTED_EDGE('',*,*,#8289,.T.);
#11504=ORIENTED_EDGE('',*,*,#8292,.T.);
#11505=ORIENTED_EDGE('',*,*,#8295,.T.);
#11506=ORIENTED_EDGE('',*,*,#8298,.T.);
#11507=ORIENTED_EDGE('',*,*,#8301,.T.);
#11508=ORIENTED_EDGE('',*,*,#8304,.T.);
#11509=ORIENTED_EDGE('',*,*,#8307,.T.);
#11510=ORIENTED_EDGE('',*,*,#8310,.T.);
#11511=ORIENTED_EDGE('',*,*,#8313,.T.);
#11512=ORIENTED_EDGE('',*,*,#8316,.T.);
#11513=ORIENTED_EDGE('',*,*,#8319,.T.);
#11514=ORIENTED_EDGE('',*,*,#8322,.T.);
#11515=ORIENTED_EDGE('',*,*,#8325,.T.);
#11516=ORIENTED_EDGE('',*,*,#8328,.T.);
#11517=ORIENTED_EDGE('',*,*,#8331,.T.);
#11518=ORIENTED_EDGE('',*,*,#8334,.T.);
#11519=ORIENTED_EDGE('',*,*,#8337,.T.);
#11520=ORIENTED_EDGE('',*,*,#8340,.T.);
#11521=ORIENTED_EDGE('',*,*,#8343,.T.);
#11522=ORIENTED_EDGE('',*,*,#8346,.T.);
#11523=ORIENTED_EDGE('',*,*,#8349,.T.);
#11524=ORIENTED_EDGE('',*,*,#8352,.T.);
#11525=ORIENTED_EDGE('',*,*,#8355,.T.);
#11526=ORIENTED_EDGE('',*,*,#8358,.T.);
#11527=ORIENTED_EDGE('',*,*,#8361,.T.);
#11528=ORIENTED_EDGE('',*,*,#8364,.T.);
#11529=ORIENTED_EDGE('',*,*,#8367,.T.);
#11530=ORIENTED_EDGE('',*,*,#8370,.T.);
#11531=ORIENTED_EDGE('',*,*,#8373,.T.);
#11532=ORIENTED_EDGE('',*,*,#8376,.T.);
#11533=ORIENTED_EDGE('',*,*,#8379,.T.);
#11534=ORIENTED_EDGE('',*,*,#8382,.T.);
#11535=ORIENTED_EDGE('',*,*,#8385,.T.);
#11536=ORIENTED_EDGE('',*,*,#8388,.T.);
#11537=ORIENTED_EDGE('',*,*,#8391,.T.);
#11538=ORIENTED_EDGE('',*,*,#8394,.T.);
#11539=ORIENTED_EDGE('',*,*,#8397,.T.);
#11540=ORIENTED_EDGE('',*,*,#8400,.T.);
#11541=ORIENTED_EDGE('',*,*,#8403,.T.);
#11542=ORIENTED_EDGE('',*,*,#8406,.T.);
#11543=ORIENTED_EDGE('',*,*,#8409,.T.);
#11544=ORIENTED_EDGE('',*,*,#8412,.T.);
#11545=ORIENTED_EDGE('',*,*,#8415,.T.);
#11546=ORIENTED_EDGE('',*,*,#8418,.T.);
#11547=ORIENTED_EDGE('',*,*,#8421,.T.);
#11548=ORIENTED_EDGE('',*,*,#8424,.T.);
#11549=ORIENTED_EDGE('',*,*,#8427,.T.);
#11550=ORIENTED_EDGE('',*,*,#8430,.T.);
#11551=ORIENTED_EDGE('',*,*,#8433,.T.);
#11552=ORIENTED_EDGE('',*,*,#8436,.T.);
#11553=ORIENTED_EDGE('',*,*,#8439,.T.);
#11554=ORIENTED_EDGE('',*,*,#8442,.T.);
#11555=ORIENTED_EDGE('',*,*,#8445,.T.);
#11556=ORIENTED_EDGE('',*,*,#8448,.T.);
#11557=ORIENTED_EDGE('',*,*,#8451,.T.);
#11558=ORIENTED_EDGE('',*,*,#8454,.T.);
#11559=ORIENTED_EDGE('',*,*,#8457,.T.);
#11560=ORIENTED_EDGE('',*,*,#8460,.T.);
#11561=ORIENTED_EDGE('',*,*,#8463,.T.);
#11562=ORIENTED_EDGE('',*,*,#8466,.T.);
#11563=ORIENTED_EDGE('',*,*,#8469,.T.);
#11564=ORIENTED_EDGE('',*,*,#8472,.T.);
#11565=ORIENTED_EDGE('',*,*,#8475,.T.);
#11566=ORIENTED_EDGE('',*,*,#8478,.T.);
#11567=ORIENTED_EDGE('',*,*,#8481,.T.);
#11568=ORIENTED_EDGE('',*,*,#8484,.T.);
#11569=ORIENTED_EDGE('',*,*,#8487,.T.);
#11570=ORIENTED_EDGE('',*,*,#8490,.T.);
#11571=ORIENTED_EDGE('',*,*,#8493,.T.);
#11572=ORIENTED_EDGE('',*,*,#8496,.T.);
#11573=ORIENTED_EDGE('',*,*,#8499,.T.);
#11574=ORIENTED_EDGE('',*,*,#8502,.T.);
#11575=ORIENTED_EDGE('',*,*,#8505,.T.);
#11576=ORIENTED_EDGE('',*,*,#8508,.T.);
#11577=ORIENTED_EDGE('',*,*,#8511,.T.);
#11578=ORIENTED_EDGE('',*,*,#8514,.T.);
#11579=ORIENTED_EDGE('',*,*,#8517,.T.);
#11580=ORIENTED_EDGE('',*,*,#8520,.T.);
#11581=ORIENTED_EDGE('',*,*,#8523,.T.);
#11582=ORIENTED_EDGE('',*,*,#8526,.T.);
#11583=ORIENTED_EDGE('',*,*,#8529,.T.);
#11584=ORIENTED_EDGE('',*,*,#8532,.T.);
#11585=ORIENTED_EDGE('',*,*,#8535,.T.);
#11586=ORIENTED_EDGE('',*,*,#8538,.T.);
#11587=ORIENTED_EDGE('',*,*,#8541,.T.);
#11588=ORIENTED_EDGE('',*,*,#8544,.T.);
#11589=ORIENTED_EDGE('',*,*,#8547,.T.);
#11590=ORIENTED_EDGE('',*,*,#8550,.T.);
#11591=ORIENTED_EDGE('',*,*,#8553,.T.);
#11592=ORIENTED_EDGE('',*,*,#8556,.T.);
#11593=ORIENTED_EDGE('',*,*,#8559,.T.);
#11594=ORIENTED_EDGE('',*,*,#8562,.T.);
#11595=ORIENTED_EDGE('',*,*,#8565,.T.);
#11596=ORIENTED_EDGE('',*,*,#8568,.T.);
#11597=ORIENTED_EDGE('',*,*,#8571,.T.);
#11598=ORIENTED_EDGE('',*,*,#8574,.T.);
#11599=ORIENTED_EDGE('',*,*,#8577,.T.);
#11600=ORIENTED_EDGE('',*,*,#8580,.T.);
#11601=ORIENTED_EDGE('',*,*,#8583,.T.);
#11602=ORIENTED_EDGE('',*,*,#8586,.T.);
#11603=ORIENTED_EDGE('',*,*,#8589,.T.);
#11604=ORIENTED_EDGE('',*,*,#8592,.T.);
#11605=ORIENTED_EDGE('',*,*,#8595,.T.);
#11606=ORIENTED_EDGE('',*,*,#8598,.T.);
#11607=ORIENTED_EDGE('',*,*,#8601,.T.);
#11608=ORIENTED_EDGE('',*,*,#8604,.T.);
#11609=ORIENTED_EDGE('',*,*,#8607,.T.);
#11610=ORIENTED_EDGE('',*,*,#8610,.T.);
#11611=ORIENTED_EDGE('',*,*,#8613,.T.);
#11612=ORIENTED_EDGE('',*,*,#8618,.F.);
#11613=ORIENTED_EDGE('',*,*,#8619,.T.);
#11614=ORIENTED_EDGE('',*,*,#8620,.F.);
#11615=ORIENTED_EDGE('',*,*,#8621,.F.);
#11616=ORIENTED_EDGE('',*,*,#8622,.T.);
#11617=ORIENTED_EDGE('',*,*,#8623,.F.);
#11618=ORIENTED_EDGE('',*,*,#8622,.F.);
#11619=ORIENTED_EDGE('',*,*,#8624,.F.);
#11620=ORIENTED_EDGE('',*,*,#8625,.F.);
#11621=ORIENTED_EDGE('',*,*,#8619,.F.);
#11622=ORIENTED_EDGE('',*,*,#8626,.F.);
#11623=ORIENTED_EDGE('',*,*,#8627,.T.);
#11624=ORIENTED_EDGE('',*,*,#8628,.F.);
#11625=ORIENTED_EDGE('',*,*,#8629,.F.);
#11626=ORIENTED_EDGE('',*,*,#8630,.T.);
#11627=ORIENTED_EDGE('',*,*,#8631,.F.);
#11628=ORIENTED_EDGE('',*,*,#8630,.F.);
#11629=ORIENTED_EDGE('',*,*,#8632,.F.);
#11630=ORIENTED_EDGE('',*,*,#8633,.F.);
#11631=ORIENTED_EDGE('',*,*,#8627,.F.);
#11632=ORIENTED_EDGE('',*,*,#8634,.F.);
#11633=ORIENTED_EDGE('',*,*,#8635,.T.);
#11634=ORIENTED_EDGE('',*,*,#8636,.F.);
#11635=ORIENTED_EDGE('',*,*,#8637,.F.);
#11636=ORIENTED_EDGE('',*,*,#8638,.T.);
#11637=ORIENTED_EDGE('',*,*,#8639,.F.);
#11638=ORIENTED_EDGE('',*,*,#8638,.F.);
#11639=ORIENTED_EDGE('',*,*,#8640,.F.);
#11640=ORIENTED_EDGE('',*,*,#8641,.F.);
#11641=ORIENTED_EDGE('',*,*,#8635,.F.);
#11642=ORIENTED_EDGE('',*,*,#8642,.F.);
#11643=ORIENTED_EDGE('',*,*,#8643,.T.);
#11644=ORIENTED_EDGE('',*,*,#8644,.F.);
#11645=ORIENTED_EDGE('',*,*,#8645,.F.);
#11646=ORIENTED_EDGE('',*,*,#8646,.T.);
#11647=ORIENTED_EDGE('',*,*,#8647,.F.);
#11648=ORIENTED_EDGE('',*,*,#8646,.F.);
#11649=ORIENTED_EDGE('',*,*,#8648,.F.);
#11650=ORIENTED_EDGE('',*,*,#8649,.F.);
#11651=ORIENTED_EDGE('',*,*,#8643,.F.);
#11652=ORIENTED_EDGE('',*,*,#8620,.T.);
#11653=ORIENTED_EDGE('',*,*,#8618,.T.);
#11654=ORIENTED_EDGE('',*,*,#8625,.T.);
#11655=ORIENTED_EDGE('',*,*,#8650,.T.);
#11656=ORIENTED_EDGE('',*,*,#8636,.T.);
#11657=ORIENTED_EDGE('',*,*,#8634,.T.);
#11658=ORIENTED_EDGE('',*,*,#8641,.T.);
#11659=ORIENTED_EDGE('',*,*,#8651,.T.);
#11660=ORIENTED_EDGE('',*,*,#8652,.F.);
#11661=ORIENTED_EDGE('',*,*,#8653,.T.);
#11662=ORIENTED_EDGE('',*,*,#8654,.F.);
#11663=ORIENTED_EDGE('',*,*,#8655,.T.);
#11664=ORIENTED_EDGE('',*,*,#8628,.T.);
#11665=ORIENTED_EDGE('',*,*,#8626,.T.);
#11666=ORIENTED_EDGE('',*,*,#8633,.T.);
#11667=ORIENTED_EDGE('',*,*,#8656,.T.);
#11668=ORIENTED_EDGE('',*,*,#8644,.T.);
#11669=ORIENTED_EDGE('',*,*,#8642,.T.);
#11670=ORIENTED_EDGE('',*,*,#8649,.T.);
#11671=ORIENTED_EDGE('',*,*,#8657,.T.);
#11672=ORIENTED_EDGE('',*,*,#8658,.F.);
#11673=ORIENTED_EDGE('',*,*,#8659,.F.);
#11674=ORIENTED_EDGE('',*,*,#8660,.F.);
#11675=ORIENTED_EDGE('',*,*,#8661,.T.);
#11676=ORIENTED_EDGE('',*,*,#8652,.T.);
#11677=ORIENTED_EDGE('',*,*,#8662,.T.);
#11678=ORIENTED_EDGE('',*,*,#8663,.T.);
#11679=ORIENTED_EDGE('',*,*,#8664,.T.);
#11680=ORIENTED_EDGE('',*,*,#8665,.T.);
#11681=ORIENTED_EDGE('',*,*,#8666,.T.);
#11682=ORIENTED_EDGE('',*,*,#8660,.T.);
#11683=ORIENTED_EDGE('',*,*,#8667,.T.);
#11684=ORIENTED_EDGE('',*,*,#8668,.T.);
#11685=ORIENTED_EDGE('',*,*,#8669,.T.);
#11686=ORIENTED_EDGE('',*,*,#8670,.T.);
#11687=ORIENTED_EDGE('',*,*,#8671,.T.);
#11688=ORIENTED_EDGE('',*,*,#8624,.T.);
#11689=ORIENTED_EDGE('',*,*,#8621,.T.);
#11690=ORIENTED_EDGE('',*,*,#8655,.F.);
#11691=ORIENTED_EDGE('',*,*,#8672,.F.);
#11692=ORIENTED_EDGE('',*,*,#8673,.F.);
#11693=ORIENTED_EDGE('',*,*,#8662,.F.);
#11694=ORIENTED_EDGE('',*,*,#8651,.F.);
#11695=ORIENTED_EDGE('',*,*,#8640,.T.);
#11696=ORIENTED_EDGE('',*,*,#8637,.T.);
#11697=ORIENTED_EDGE('',*,*,#8650,.F.);
#11698=ORIENTED_EDGE('',*,*,#8673,.T.);
#11699=ORIENTED_EDGE('',*,*,#8674,.F.);
#11700=ORIENTED_EDGE('',*,*,#8675,.F.);
#11701=ORIENTED_EDGE('',*,*,#8663,.F.);
#11702=ORIENTED_EDGE('',*,*,#8675,.T.);
#11703=ORIENTED_EDGE('',*,*,#8676,.F.);
#11704=ORIENTED_EDGE('',*,*,#8677,.F.);
#11705=ORIENTED_EDGE('',*,*,#8664,.F.);
#11706=ORIENTED_EDGE('',*,*,#8623,.T.);
#11707=ORIENTED_EDGE('',*,*,#8631,.T.);
#11708=ORIENTED_EDGE('',*,*,#8639,.T.);
#11709=ORIENTED_EDGE('',*,*,#8647,.T.);
#11710=ORIENTED_EDGE('',*,*,#8677,.T.);
#11711=ORIENTED_EDGE('',*,*,#8678,.F.);
#11712=ORIENTED_EDGE('',*,*,#8679,.F.);
#11713=ORIENTED_EDGE('',*,*,#8665,.F.);
#11714=ORIENTED_EDGE('',*,*,#8632,.T.);
#11715=ORIENTED_EDGE('',*,*,#8629,.T.);
#11716=ORIENTED_EDGE('',*,*,#8661,.F.);
#11717=ORIENTED_EDGE('',*,*,#8666,.F.);
#11718=ORIENTED_EDGE('',*,*,#8679,.T.);
#11719=ORIENTED_EDGE('',*,*,#8680,.F.);
#11720=ORIENTED_EDGE('',*,*,#8657,.F.);
#11721=ORIENTED_EDGE('',*,*,#8648,.T.);
#11722=ORIENTED_EDGE('',*,*,#8645,.T.);
#11723=ORIENTED_EDGE('',*,*,#8656,.F.);
#11724=ORIENTED_EDGE('',*,*,#8659,.T.);
#11725=ORIENTED_EDGE('',*,*,#8681,.F.);
#11726=ORIENTED_EDGE('',*,*,#8682,.F.);
#11727=ORIENTED_EDGE('',*,*,#8667,.F.);
#11728=ORIENTED_EDGE('',*,*,#8682,.T.);
#11729=ORIENTED_EDGE('',*,*,#8683,.F.);
#11730=ORIENTED_EDGE('',*,*,#8684,.F.);
#11731=ORIENTED_EDGE('',*,*,#8668,.F.);
#11732=ORIENTED_EDGE('',*,*,#8684,.T.);
#11733=ORIENTED_EDGE('',*,*,#8685,.F.);
#11734=ORIENTED_EDGE('',*,*,#8686,.F.);
#11735=ORIENTED_EDGE('',*,*,#8669,.F.);
#11736=ORIENTED_EDGE('',*,*,#8686,.T.);
#11737=ORIENTED_EDGE('',*,*,#8687,.F.);
#11738=ORIENTED_EDGE('',*,*,#8688,.F.);
#11739=ORIENTED_EDGE('',*,*,#8670,.F.);
#11740=ORIENTED_EDGE('',*,*,#8688,.T.);
#11741=ORIENTED_EDGE('',*,*,#8689,.F.);
#11742=ORIENTED_EDGE('',*,*,#8653,.F.);
#11743=ORIENTED_EDGE('',*,*,#8671,.F.);
#11744=ORIENTED_EDGE('',*,*,#8654,.T.);
#11745=ORIENTED_EDGE('',*,*,#8689,.T.);
#11746=ORIENTED_EDGE('',*,*,#8687,.T.);
#11747=ORIENTED_EDGE('',*,*,#8685,.T.);
#11748=ORIENTED_EDGE('',*,*,#8683,.T.);
#11749=ORIENTED_EDGE('',*,*,#8681,.T.);
#11750=ORIENTED_EDGE('',*,*,#8658,.T.);
#11751=ORIENTED_EDGE('',*,*,#8680,.T.);
#11752=ORIENTED_EDGE('',*,*,#8678,.T.);
#11753=ORIENTED_EDGE('',*,*,#8676,.T.);
#11754=ORIENTED_EDGE('',*,*,#8674,.T.);
#11755=ORIENTED_EDGE('',*,*,#8672,.T.);
#11756=ORIENTED_EDGE('',*,*,#8690,.T.);
#11757=ORIENTED_EDGE('',*,*,#8691,.T.);
#11758=ORIENTED_EDGE('',*,*,#8692,.F.);
#11759=ORIENTED_EDGE('',*,*,#8693,.F.);
#11760=ORIENTED_EDGE('',*,*,#8694,.T.);
#11761=ORIENTED_EDGE('',*,*,#8693,.T.);
#11762=ORIENTED_EDGE('',*,*,#8695,.F.);
#11763=ORIENTED_EDGE('',*,*,#8696,.F.);
#11764=ORIENTED_EDGE('',*,*,#8697,.T.);
#11765=ORIENTED_EDGE('',*,*,#8696,.T.);
#11766=ORIENTED_EDGE('',*,*,#8698,.F.);
#11767=ORIENTED_EDGE('',*,*,#8699,.F.);
#11768=ORIENTED_EDGE('',*,*,#8700,.T.);
#11769=ORIENTED_EDGE('',*,*,#8699,.T.);
#11770=ORIENTED_EDGE('',*,*,#8701,.F.);
#11771=ORIENTED_EDGE('',*,*,#8702,.F.);
#11772=ORIENTED_EDGE('',*,*,#8703,.T.);
#11773=ORIENTED_EDGE('',*,*,#8702,.T.);
#11774=ORIENTED_EDGE('',*,*,#8704,.F.);
#11775=ORIENTED_EDGE('',*,*,#8705,.F.);
#11776=ORIENTED_EDGE('',*,*,#8706,.T.);
#11777=ORIENTED_EDGE('',*,*,#8705,.T.);
#11778=ORIENTED_EDGE('',*,*,#8707,.F.);
#11779=ORIENTED_EDGE('',*,*,#8708,.F.);
#11780=ORIENTED_EDGE('',*,*,#8709,.T.);
#11781=ORIENTED_EDGE('',*,*,#8708,.T.);
#11782=ORIENTED_EDGE('',*,*,#8710,.F.);
#11783=ORIENTED_EDGE('',*,*,#8711,.F.);
#11784=ORIENTED_EDGE('',*,*,#8712,.T.);
#11785=ORIENTED_EDGE('',*,*,#8711,.T.);
#11786=ORIENTED_EDGE('',*,*,#8713,.F.);
#11787=ORIENTED_EDGE('',*,*,#8691,.F.);
#11788=ORIENTED_EDGE('',*,*,#8713,.T.);
#11789=ORIENTED_EDGE('',*,*,#8710,.T.);
#11790=ORIENTED_EDGE('',*,*,#8707,.T.);
#11791=ORIENTED_EDGE('',*,*,#8704,.T.);
#11792=ORIENTED_EDGE('',*,*,#8701,.T.);
#11793=ORIENTED_EDGE('',*,*,#8698,.T.);
#11794=ORIENTED_EDGE('',*,*,#8695,.T.);
#11795=ORIENTED_EDGE('',*,*,#8692,.T.);
#11796=ORIENTED_EDGE('',*,*,#8712,.F.);
#11797=ORIENTED_EDGE('',*,*,#8690,.F.);
#11798=ORIENTED_EDGE('',*,*,#8694,.F.);
#11799=ORIENTED_EDGE('',*,*,#8697,.F.);
#11800=ORIENTED_EDGE('',*,*,#8700,.F.);
#11801=ORIENTED_EDGE('',*,*,#8703,.F.);
#11802=ORIENTED_EDGE('',*,*,#8706,.F.);
#11803=ORIENTED_EDGE('',*,*,#8709,.F.);
#11804=ORIENTED_EDGE('',*,*,#8714,.F.);
#11805=ORIENTED_EDGE('',*,*,#8715,.T.);
#11806=ORIENTED_EDGE('',*,*,#8716,.F.);
#11807=ORIENTED_EDGE('',*,*,#8717,.F.);
#11808=ORIENTED_EDGE('',*,*,#8718,.F.);
#11809=ORIENTED_EDGE('',*,*,#8717,.T.);
#11810=ORIENTED_EDGE('',*,*,#8719,.F.);
#11811=ORIENTED_EDGE('',*,*,#8720,.F.);
#11812=ORIENTED_EDGE('',*,*,#8721,.F.);
#11813=ORIENTED_EDGE('',*,*,#8720,.T.);
#11814=ORIENTED_EDGE('',*,*,#8722,.F.);
#11815=ORIENTED_EDGE('',*,*,#8723,.F.);
#11816=ORIENTED_EDGE('',*,*,#8724,.F.);
#11817=ORIENTED_EDGE('',*,*,#8723,.T.);
#11818=ORIENTED_EDGE('',*,*,#8725,.F.);
#11819=ORIENTED_EDGE('',*,*,#8726,.F.);
#11820=ORIENTED_EDGE('',*,*,#8727,.F.);
#11821=ORIENTED_EDGE('',*,*,#8726,.T.);
#11822=ORIENTED_EDGE('',*,*,#8728,.F.);
#11823=ORIENTED_EDGE('',*,*,#8729,.F.);
#11824=ORIENTED_EDGE('',*,*,#8730,.F.);
#11825=ORIENTED_EDGE('',*,*,#8729,.T.);
#11826=ORIENTED_EDGE('',*,*,#8731,.F.);
#11827=ORIENTED_EDGE('',*,*,#8732,.F.);
#11828=ORIENTED_EDGE('',*,*,#8733,.F.);
#11829=ORIENTED_EDGE('',*,*,#8732,.T.);
#11830=ORIENTED_EDGE('',*,*,#8734,.F.);
#11831=ORIENTED_EDGE('',*,*,#8735,.F.);
#11832=ORIENTED_EDGE('',*,*,#8736,.F.);
#11833=ORIENTED_EDGE('',*,*,#8735,.T.);
#11834=ORIENTED_EDGE('',*,*,#8737,.F.);
#11835=ORIENTED_EDGE('',*,*,#8715,.F.);
#11836=ORIENTED_EDGE('',*,*,#8736,.T.);
#11837=ORIENTED_EDGE('',*,*,#8714,.T.);
#11838=ORIENTED_EDGE('',*,*,#8718,.T.);
#11839=ORIENTED_EDGE('',*,*,#8721,.T.);
#11840=ORIENTED_EDGE('',*,*,#8724,.T.);
#11841=ORIENTED_EDGE('',*,*,#8727,.T.);
#11842=ORIENTED_EDGE('',*,*,#8730,.T.);
#11843=ORIENTED_EDGE('',*,*,#8733,.T.);
#11844=ORIENTED_EDGE('',*,*,#8737,.T.);
#11845=ORIENTED_EDGE('',*,*,#8734,.T.);
#11846=ORIENTED_EDGE('',*,*,#8731,.T.);
#11847=ORIENTED_EDGE('',*,*,#8728,.T.);
#11848=ORIENTED_EDGE('',*,*,#8725,.T.);
#11849=ORIENTED_EDGE('',*,*,#8722,.T.);
#11850=ORIENTED_EDGE('',*,*,#8719,.T.);
#11851=ORIENTED_EDGE('',*,*,#8716,.T.);
#11852=ORIENTED_EDGE('',*,*,#8738,.T.);
#11853=ORIENTED_EDGE('',*,*,#8739,.T.);
#11854=ORIENTED_EDGE('',*,*,#8740,.T.);
#11855=ORIENTED_EDGE('',*,*,#8741,.F.);
#11856=ORIENTED_EDGE('',*,*,#8742,.T.);
#11857=ORIENTED_EDGE('',*,*,#8743,.T.);
#11858=ORIENTED_EDGE('',*,*,#8744,.T.);
#11859=ORIENTED_EDGE('',*,*,#8739,.F.);
#11860=ORIENTED_EDGE('',*,*,#8745,.T.);
#11861=ORIENTED_EDGE('',*,*,#8746,.T.);
#11862=ORIENTED_EDGE('',*,*,#8747,.T.);
#11863=ORIENTED_EDGE('',*,*,#8743,.F.);
#11864=ORIENTED_EDGE('',*,*,#8748,.T.);
#11865=ORIENTED_EDGE('',*,*,#8749,.T.);
#11866=ORIENTED_EDGE('',*,*,#8750,.T.);
#11867=ORIENTED_EDGE('',*,*,#8746,.F.);
#11868=ORIENTED_EDGE('',*,*,#8751,.T.);
#11869=ORIENTED_EDGE('',*,*,#8752,.T.);
#11870=ORIENTED_EDGE('',*,*,#8753,.T.);
#11871=ORIENTED_EDGE('',*,*,#8749,.F.);
#11872=ORIENTED_EDGE('',*,*,#8754,.T.);
#11873=ORIENTED_EDGE('',*,*,#8741,.T.);
#11874=ORIENTED_EDGE('',*,*,#8755,.T.);
#11875=ORIENTED_EDGE('',*,*,#8752,.F.);
#11876=ORIENTED_EDGE('',*,*,#8754,.F.);
#11877=ORIENTED_EDGE('',*,*,#8751,.F.);
#11878=ORIENTED_EDGE('',*,*,#8748,.F.);
#11879=ORIENTED_EDGE('',*,*,#8745,.F.);
#11880=ORIENTED_EDGE('',*,*,#8742,.F.);
#11881=ORIENTED_EDGE('',*,*,#8738,.F.);
#11882=ORIENTED_EDGE('',*,*,#8755,.F.);
#11883=ORIENTED_EDGE('',*,*,#8740,.F.);
#11884=ORIENTED_EDGE('',*,*,#8744,.F.);
#11885=ORIENTED_EDGE('',*,*,#8747,.F.);
#11886=ORIENTED_EDGE('',*,*,#8750,.F.);
#11887=ORIENTED_EDGE('',*,*,#8753,.F.);
#11888=ORIENTED_EDGE('',*,*,#8756,.F.);
#11889=ORIENTED_EDGE('',*,*,#8757,.F.);
#11890=ORIENTED_EDGE('',*,*,#8758,.F.);
#11891=ORIENTED_EDGE('',*,*,#8759,.T.);
#11892=ORIENTED_EDGE('',*,*,#8757,.T.);
#11893=ORIENTED_EDGE('',*,*,#8759,.F.);
#11894=ORIENTED_EDGE('',*,*,#8760,.F.);
#11895=ORIENTED_EDGE('',*,*,#8761,.T.);
#11896=ORIENTED_EDGE('',*,*,#8758,.T.);
#11897=ORIENTED_EDGE('',*,*,#8761,.F.);
#11898=ORIENTED_EDGE('',*,*,#8762,.F.);
#11899=ORIENTED_EDGE('',*,*,#8763,.T.);
#11900=ORIENTED_EDGE('',*,*,#8760,.T.);
#11901=ORIENTED_EDGE('',*,*,#8763,.F.);
#11902=ORIENTED_EDGE('',*,*,#8762,.T.);
#11903=ORIENTED_EDGE('',*,*,#8764,.F.);
#11904=ORIENTED_EDGE('',*,*,#8765,.F.);
#11905=ORIENTED_EDGE('',*,*,#8766,.T.);
#11906=ORIENTED_EDGE('',*,*,#8764,.T.);
#11907=ORIENTED_EDGE('',*,*,#8766,.F.);
#11908=ORIENTED_EDGE('',*,*,#8756,.T.);
#11909=ORIENTED_EDGE('',*,*,#8767,.T.);
#11910=ORIENTED_EDGE('',*,*,#8765,.T.);
#11911=ORIENTED_EDGE('',*,*,#8767,.F.);
#11912=ORIENTED_EDGE('',*,*,#8768,.F.);
#11913=ORIENTED_EDGE('',*,*,#8769,.T.);
#11914=ORIENTED_EDGE('',*,*,#8770,.F.);
#11915=ORIENTED_EDGE('',*,*,#8771,.T.);
#11916=ORIENTED_EDGE('',*,*,#8772,.F.);
#11917=ORIENTED_EDGE('',*,*,#8771,.F.);
#11918=ORIENTED_EDGE('',*,*,#8773,.F.);
#11919=ORIENTED_EDGE('',*,*,#8774,.F.);
#11920=ORIENTED_EDGE('',*,*,#8775,.F.);
#11921=ORIENTED_EDGE('',*,*,#8774,.T.);
#11922=ORIENTED_EDGE('',*,*,#8776,.T.);
#11923=ORIENTED_EDGE('',*,*,#8777,.T.);
#11924=ORIENTED_EDGE('',*,*,#8773,.T.);
#11925=ORIENTED_EDGE('',*,*,#8770,.T.);
#11926=ORIENTED_EDGE('',*,*,#8778,.T.);
#11927=ORIENTED_EDGE('',*,*,#8776,.F.);
#11928=ORIENTED_EDGE('',*,*,#8779,.F.);
#11929=ORIENTED_EDGE('',*,*,#8777,.F.);
#11930=ORIENTED_EDGE('',*,*,#8778,.F.);
#11931=ORIENTED_EDGE('',*,*,#8769,.F.);
#11932=ORIENTED_EDGE('',*,*,#8780,.F.);
#11933=ORIENTED_EDGE('',*,*,#8781,.T.);
#11934=ORIENTED_EDGE('',*,*,#8782,.F.);
#11935=ORIENTED_EDGE('',*,*,#8781,.F.);
#11936=ORIENTED_EDGE('',*,*,#8780,.T.);
#11937=ORIENTED_EDGE('',*,*,#8783,.F.);
#11938=ORIENTED_EDGE('',*,*,#8784,.T.);
#11939=ORIENTED_EDGE('',*,*,#8785,.T.);
#11940=ORIENTED_EDGE('',*,*,#8784,.F.);
#11941=ORIENTED_EDGE('',*,*,#8785,.F.);
#11942=ORIENTED_EDGE('',*,*,#8786,.F.);
#11943=ORIENTED_EDGE('',*,*,#8787,.T.);
#11944=ORIENTED_EDGE('',*,*,#8788,.F.);
#11945=ORIENTED_EDGE('',*,*,#8789,.T.);
#11946=ORIENTED_EDGE('',*,*,#8790,.F.);
#11947=ORIENTED_EDGE('',*,*,#8789,.F.);
#11948=ORIENTED_EDGE('',*,*,#8791,.F.);
#11949=ORIENTED_EDGE('',*,*,#8792,.F.);
#11950=ORIENTED_EDGE('',*,*,#8793,.F.);
#11951=ORIENTED_EDGE('',*,*,#8792,.T.);
#11952=ORIENTED_EDGE('',*,*,#8794,.T.);
#11953=ORIENTED_EDGE('',*,*,#8795,.T.);
#11954=ORIENTED_EDGE('',*,*,#8791,.T.);
#11955=ORIENTED_EDGE('',*,*,#8788,.T.);
#11956=ORIENTED_EDGE('',*,*,#8796,.T.);
#11957=ORIENTED_EDGE('',*,*,#8794,.F.);
#11958=ORIENTED_EDGE('',*,*,#8797,.F.);
#11959=ORIENTED_EDGE('',*,*,#8795,.F.);
#11960=ORIENTED_EDGE('',*,*,#8796,.F.);
#11961=ORIENTED_EDGE('',*,*,#8787,.F.);
#11962=ORIENTED_EDGE('',*,*,#8798,.T.);
#11963=ORIENTED_EDGE('',*,*,#8799,.F.);
#11964=ORIENTED_EDGE('',*,*,#8800,.F.);
#11965=ORIENTED_EDGE('',*,*,#8801,.F.);
#11966=ORIENTED_EDGE('',*,*,#8798,.F.);
#11967=ORIENTED_EDGE('',*,*,#8802,.T.);
#11968=ORIENTED_EDGE('',*,*,#8800,.T.);
#11969=ORIENTED_EDGE('',*,*,#8802,.F.);
#11970=ORIENTED_EDGE('',*,*,#8801,.T.);
#11971=ORIENTED_EDGE('',*,*,#8803,.T.);
#11972=ORIENTED_EDGE('',*,*,#8804,.T.);
#11973=ORIENTED_EDGE('',*,*,#8803,.F.);
#11974=ORIENTED_EDGE('',*,*,#8805,.F.);
#11975=ORIENTED_EDGE('',*,*,#8806,.T.);
#11976=ORIENTED_EDGE('',*,*,#8799,.T.);
#11977=ORIENTED_EDGE('',*,*,#8806,.F.);
#11978=ORIENTED_EDGE('',*,*,#8775,.T.);
#11979=ORIENTED_EDGE('',*,*,#8779,.T.);
#11980=ORIENTED_EDGE('',*,*,#8768,.T.);
#11981=ORIENTED_EDGE('',*,*,#8772,.T.);
#11982=ORIENTED_EDGE('',*,*,#8793,.T.);
#11983=ORIENTED_EDGE('',*,*,#8797,.T.);
#11984=ORIENTED_EDGE('',*,*,#8786,.T.);
#11985=ORIENTED_EDGE('',*,*,#8790,.T.);
#11986=ORIENTED_EDGE('',*,*,#8805,.T.);
#11987=ORIENTED_EDGE('',*,*,#8782,.T.);
#11988=ORIENTED_EDGE('',*,*,#8804,.F.);
#11989=ORIENTED_EDGE('',*,*,#8783,.T.);
#11990=ORIENTED_EDGE('',*,*,#8807,.F.);
#11991=ORIENTED_EDGE('',*,*,#8808,.T.);
#11992=ORIENTED_EDGE('',*,*,#8809,.T.);
#11993=ORIENTED_EDGE('',*,*,#8808,.F.);
#11994=ORIENTED_EDGE('',*,*,#8810,.F.);
#11995=ORIENTED_EDGE('',*,*,#8811,.T.);
#11996=ORIENTED_EDGE('',*,*,#8812,.T.);
#11997=ORIENTED_EDGE('',*,*,#8811,.F.);
#11998=ORIENTED_EDGE('',*,*,#8810,.T.);
#11999=ORIENTED_EDGE('',*,*,#8807,.T.);
#12000=ORIENTED_EDGE('',*,*,#8812,.F.);
#12001=ORIENTED_EDGE('',*,*,#8809,.F.);
#12002=ORIENTED_EDGE('',*,*,#8813,.F.);
#12003=ORIENTED_EDGE('',*,*,#8814,.T.);
#12004=ORIENTED_EDGE('',*,*,#8815,.T.);
#12005=ORIENTED_EDGE('',*,*,#8814,.F.);
#12006=ORIENTED_EDGE('',*,*,#8816,.F.);
#12007=ORIENTED_EDGE('',*,*,#8817,.T.);
#12008=ORIENTED_EDGE('',*,*,#8818,.T.);
#12009=ORIENTED_EDGE('',*,*,#8817,.F.);
#12010=ORIENTED_EDGE('',*,*,#8816,.T.);
#12011=ORIENTED_EDGE('',*,*,#8813,.T.);
#12012=ORIENTED_EDGE('',*,*,#8818,.F.);
#12013=ORIENTED_EDGE('',*,*,#8815,.F.);
#12014=ORIENTED_EDGE('',*,*,#8819,.F.);
#12015=ORIENTED_EDGE('',*,*,#8820,.T.);
#12016=ORIENTED_EDGE('',*,*,#8821,.T.);
#12017=ORIENTED_EDGE('',*,*,#8820,.F.);
#12018=ORIENTED_EDGE('',*,*,#8822,.F.);
#12019=ORIENTED_EDGE('',*,*,#8823,.T.);
#12020=ORIENTED_EDGE('',*,*,#8824,.T.);
#12021=ORIENTED_EDGE('',*,*,#8823,.F.);
#12022=ORIENTED_EDGE('',*,*,#8822,.T.);
#12023=ORIENTED_EDGE('',*,*,#8819,.T.);
#12024=ORIENTED_EDGE('',*,*,#8824,.F.);
#12025=ORIENTED_EDGE('',*,*,#8821,.F.);
#12026=ORIENTED_EDGE('',*,*,#8825,.F.);
#12027=ORIENTED_EDGE('',*,*,#8826,.T.);
#12028=ORIENTED_EDGE('',*,*,#8827,.T.);
#12029=ORIENTED_EDGE('',*,*,#8826,.F.);
#12030=ORIENTED_EDGE('',*,*,#8828,.F.);
#12031=ORIENTED_EDGE('',*,*,#8829,.T.);
#12032=ORIENTED_EDGE('',*,*,#8830,.T.);
#12033=ORIENTED_EDGE('',*,*,#8829,.F.);
#12034=ORIENTED_EDGE('',*,*,#8828,.T.);
#12035=ORIENTED_EDGE('',*,*,#8825,.T.);
#12036=ORIENTED_EDGE('',*,*,#8830,.F.);
#12037=ORIENTED_EDGE('',*,*,#8827,.F.);
#12038=ORIENTED_EDGE('',*,*,#8831,.F.);
#12039=ORIENTED_EDGE('',*,*,#8832,.T.);
#12040=ORIENTED_EDGE('',*,*,#8833,.T.);
#12041=ORIENTED_EDGE('',*,*,#8832,.F.);
#12042=ORIENTED_EDGE('',*,*,#8834,.F.);
#12043=ORIENTED_EDGE('',*,*,#8835,.T.);
#12044=ORIENTED_EDGE('',*,*,#8836,.T.);
#12045=ORIENTED_EDGE('',*,*,#8835,.F.);
#12046=ORIENTED_EDGE('',*,*,#8834,.T.);
#12047=ORIENTED_EDGE('',*,*,#8831,.T.);
#12048=ORIENTED_EDGE('',*,*,#8836,.F.);
#12049=ORIENTED_EDGE('',*,*,#8833,.F.);
#12050=ORIENTED_EDGE('',*,*,#8837,.F.);
#12051=ORIENTED_EDGE('',*,*,#8838,.T.);
#12052=ORIENTED_EDGE('',*,*,#8839,.T.);
#12053=ORIENTED_EDGE('',*,*,#8838,.F.);
#12054=ORIENTED_EDGE('',*,*,#8840,.F.);
#12055=ORIENTED_EDGE('',*,*,#8841,.T.);
#12056=ORIENTED_EDGE('',*,*,#8842,.T.);
#12057=ORIENTED_EDGE('',*,*,#8841,.F.);
#12058=ORIENTED_EDGE('',*,*,#8840,.T.);
#12059=ORIENTED_EDGE('',*,*,#8837,.T.);
#12060=ORIENTED_EDGE('',*,*,#8842,.F.);
#12061=ORIENTED_EDGE('',*,*,#8839,.F.);
#12062=ORIENTED_EDGE('',*,*,#8843,.F.);
#12063=ORIENTED_EDGE('',*,*,#8844,.T.);
#12064=ORIENTED_EDGE('',*,*,#8845,.F.);
#12065=ORIENTED_EDGE('',*,*,#8844,.F.);
#12066=ORIENTED_EDGE('',*,*,#8846,.F.);
#12067=ORIENTED_EDGE('',*,*,#8847,.T.);
#12068=ORIENTED_EDGE('',*,*,#8848,.F.);
#12069=ORIENTED_EDGE('',*,*,#8849,.F.);
#12070=ORIENTED_EDGE('',*,*,#8850,.F.);
#12071=ORIENTED_EDGE('',*,*,#8851,.T.);
#12072=ORIENTED_EDGE('',*,*,#8852,.F.);
#12073=ORIENTED_EDGE('',*,*,#8847,.F.);
#12074=ORIENTED_EDGE('',*,*,#8853,.F.);
#12075=ORIENTED_EDGE('',*,*,#8854,.F.);
#12076=ORIENTED_EDGE('',*,*,#8855,.F.);
#12077=ORIENTED_EDGE('',*,*,#8851,.F.);
#12078=ORIENTED_EDGE('',*,*,#8856,.T.);
#12079=ORIENTED_EDGE('',*,*,#8848,.T.);
#12080=ORIENTED_EDGE('',*,*,#8852,.T.);
#12081=ORIENTED_EDGE('',*,*,#8855,.T.);
#12082=ORIENTED_EDGE('',*,*,#8857,.T.);
#12083=ORIENTED_EDGE('',*,*,#8849,.T.);
#12084=ORIENTED_EDGE('',*,*,#8857,.F.);
#12085=ORIENTED_EDGE('',*,*,#8854,.T.);
#12086=ORIENTED_EDGE('',*,*,#8858,.T.);
#12087=ORIENTED_EDGE('',*,*,#8859,.F.);
#12088=ORIENTED_EDGE('',*,*,#8860,.F.);
#12089=ORIENTED_EDGE('',*,*,#8861,.F.);
#12090=ORIENTED_EDGE('',*,*,#8862,.T.);
#12091=ORIENTED_EDGE('',*,*,#8859,.T.);
#12092=ORIENTED_EDGE('',*,*,#8863,.F.);
#12093=ORIENTED_EDGE('',*,*,#8864,.F.);
#12094=ORIENTED_EDGE('',*,*,#8865,.F.);
#12095=ORIENTED_EDGE('',*,*,#8862,.F.);
#12096=ORIENTED_EDGE('',*,*,#8866,.T.);
#12097=ORIENTED_EDGE('',*,*,#8867,.F.);
#12098=ORIENTED_EDGE('',*,*,#8863,.T.);
#12099=ORIENTED_EDGE('',*,*,#8843,.T.);
#12100=ORIENTED_EDGE('',*,*,#8861,.T.);
#12101=ORIENTED_EDGE('',*,*,#8868,.F.);
#12102=ORIENTED_EDGE('',*,*,#8869,.F.);
#12103=ORIENTED_EDGE('',*,*,#8866,.F.);
#12104=ORIENTED_EDGE('',*,*,#8865,.T.);
#12105=ORIENTED_EDGE('',*,*,#8870,.F.);
#12106=ORIENTED_EDGE('',*,*,#8868,.T.);
#12107=ORIENTED_EDGE('',*,*,#8860,.T.);
#12108=ORIENTED_EDGE('',*,*,#8845,.T.);
#12109=ORIENTED_EDGE('',*,*,#8856,.F.);
#12110=ORIENTED_EDGE('',*,*,#8871,.T.);
#12111=ORIENTED_EDGE('',*,*,#8872,.T.);
#12112=ORIENTED_EDGE('',*,*,#8871,.F.);
#12113=ORIENTED_EDGE('',*,*,#8864,.T.);
#12114=ORIENTED_EDGE('',*,*,#8867,.T.);
#12115=ORIENTED_EDGE('',*,*,#8869,.T.);
#12116=ORIENTED_EDGE('',*,*,#8870,.T.);
#12117=ORIENTED_EDGE('',*,*,#8872,.F.);
#12118=ORIENTED_EDGE('',*,*,#8846,.T.);
#12119=ORIENTED_EDGE('',*,*,#8858,.F.);
#12120=ORIENTED_EDGE('',*,*,#8853,.T.);
#12121=ORIENTED_EDGE('',*,*,#8850,.T.);
#12122=ORIENTED_EDGE('',*,*,#8873,.F.);
#12123=ORIENTED_EDGE('',*,*,#8874,.T.);
#12124=ORIENTED_EDGE('',*,*,#8875,.T.);
#12125=ORIENTED_EDGE('',*,*,#8874,.F.);
#12126=ORIENTED_EDGE('',*,*,#8876,.F.);
#12127=ORIENTED_EDGE('',*,*,#8877,.T.);
#12128=ORIENTED_EDGE('',*,*,#8878,.T.);
#12129=ORIENTED_EDGE('',*,*,#8877,.F.);
#12130=ORIENTED_EDGE('',*,*,#8876,.T.);
#12131=ORIENTED_EDGE('',*,*,#8873,.T.);
#12132=ORIENTED_EDGE('',*,*,#8878,.F.);
#12133=ORIENTED_EDGE('',*,*,#8875,.F.);
#12134=ORIENTED_EDGE('',*,*,#8879,.F.);
#12135=ORIENTED_EDGE('',*,*,#8880,.F.);
#12136=ORIENTED_EDGE('',*,*,#8881,.F.);
#12137=ORIENTED_EDGE('',*,*,#8882,.F.);
#12138=ORIENTED_EDGE('',*,*,#8883,.F.);
#12139=ORIENTED_EDGE('',*,*,#8884,.T.);
#12140=ORIENTED_EDGE('',*,*,#8885,.F.);
#12141=ORIENTED_EDGE('',*,*,#8880,.T.);
#12142=ORIENTED_EDGE('',*,*,#8886,.F.);
#12143=ORIENTED_EDGE('',*,*,#8887,.F.);
#12144=ORIENTED_EDGE('',*,*,#8888,.F.);
#12145=ORIENTED_EDGE('',*,*,#8884,.F.);
#12146=ORIENTED_EDGE('',*,*,#8889,.T.);
#12147=ORIENTED_EDGE('',*,*,#8890,.T.);
#12148=ORIENTED_EDGE('',*,*,#8891,.T.);
#12149=ORIENTED_EDGE('',*,*,#8892,.T.);
#12150=ORIENTED_EDGE('',*,*,#8893,.T.);
#12151=ORIENTED_EDGE('',*,*,#8894,.T.);
#12152=ORIENTED_EDGE('',*,*,#8895,.T.);
#12153=ORIENTED_EDGE('',*,*,#8896,.T.);
#12154=ORIENTED_EDGE('',*,*,#8897,.T.);
#12155=ORIENTED_EDGE('',*,*,#8898,.T.);
#12156=ORIENTED_EDGE('',*,*,#8899,.T.);
#12157=ORIENTED_EDGE('',*,*,#8900,.T.);
#12158=ORIENTED_EDGE('',*,*,#8901,.T.);
#12159=ORIENTED_EDGE('',*,*,#8902,.T.);
#12160=ORIENTED_EDGE('',*,*,#8903,.T.);
#12161=ORIENTED_EDGE('',*,*,#8904,.T.);
#12162=ORIENTED_EDGE('',*,*,#8905,.T.);
#12163=ORIENTED_EDGE('',*,*,#8906,.T.);
#12164=ORIENTED_EDGE('',*,*,#8907,.T.);
#12165=ORIENTED_EDGE('',*,*,#8908,.T.);
#12166=ORIENTED_EDGE('',*,*,#8909,.T.);
#12167=ORIENTED_EDGE('',*,*,#8910,.T.);
#12168=ORIENTED_EDGE('',*,*,#8911,.T.);
#12169=ORIENTED_EDGE('',*,*,#8912,.T.);
#12170=ORIENTED_EDGE('',*,*,#8913,.T.);
#12171=ORIENTED_EDGE('',*,*,#8914,.T.);
#12172=ORIENTED_EDGE('',*,*,#8915,.T.);
#12173=ORIENTED_EDGE('',*,*,#8916,.T.);
#12174=ORIENTED_EDGE('',*,*,#8917,.T.);
#12175=ORIENTED_EDGE('',*,*,#8918,.T.);
#12176=ORIENTED_EDGE('',*,*,#8919,.T.);
#12177=ORIENTED_EDGE('',*,*,#8920,.T.);
#12178=ORIENTED_EDGE('',*,*,#8921,.T.);
#12179=ORIENTED_EDGE('',*,*,#8922,.T.);
#12180=ORIENTED_EDGE('',*,*,#8923,.T.);
#12181=ORIENTED_EDGE('',*,*,#8924,.T.);
#12182=ORIENTED_EDGE('',*,*,#8925,.T.);
#12183=ORIENTED_EDGE('',*,*,#8926,.T.);
#12184=ORIENTED_EDGE('',*,*,#8927,.T.);
#12185=ORIENTED_EDGE('',*,*,#8928,.T.);
#12186=ORIENTED_EDGE('',*,*,#8929,.T.);
#12187=ORIENTED_EDGE('',*,*,#8930,.T.);
#12188=ORIENTED_EDGE('',*,*,#8931,.T.);
#12189=ORIENTED_EDGE('',*,*,#8932,.T.);
#12190=ORIENTED_EDGE('',*,*,#8933,.T.);
#12191=ORIENTED_EDGE('',*,*,#8934,.T.);
#12192=ORIENTED_EDGE('',*,*,#8935,.T.);
#12193=ORIENTED_EDGE('',*,*,#8936,.T.);
#12194=ORIENTED_EDGE('',*,*,#8937,.T.);
#12195=ORIENTED_EDGE('',*,*,#8938,.T.);
#12196=ORIENTED_EDGE('',*,*,#8939,.T.);
#12197=ORIENTED_EDGE('',*,*,#8940,.T.);
#12198=ORIENTED_EDGE('',*,*,#8941,.T.);
#12199=ORIENTED_EDGE('',*,*,#8942,.T.);
#12200=ORIENTED_EDGE('',*,*,#8943,.T.);
#12201=ORIENTED_EDGE('',*,*,#8944,.T.);
#12202=ORIENTED_EDGE('',*,*,#8945,.T.);
#12203=ORIENTED_EDGE('',*,*,#8946,.T.);
#12204=ORIENTED_EDGE('',*,*,#8947,.T.);
#12205=ORIENTED_EDGE('',*,*,#8948,.T.);
#12206=ORIENTED_EDGE('',*,*,#8949,.T.);
#12207=ORIENTED_EDGE('',*,*,#8950,.T.);
#12208=ORIENTED_EDGE('',*,*,#8951,.T.);
#12209=ORIENTED_EDGE('',*,*,#8952,.T.);
#12210=ORIENTED_EDGE('',*,*,#8953,.T.);
#12211=ORIENTED_EDGE('',*,*,#8954,.T.);
#12212=ORIENTED_EDGE('',*,*,#8955,.T.);
#12213=ORIENTED_EDGE('',*,*,#8956,.T.);
#12214=ORIENTED_EDGE('',*,*,#8957,.T.);
#12215=ORIENTED_EDGE('',*,*,#8958,.T.);
#12216=ORIENTED_EDGE('',*,*,#8959,.T.);
#12217=ORIENTED_EDGE('',*,*,#8960,.T.);
#12218=ORIENTED_EDGE('',*,*,#8961,.T.);
#12219=ORIENTED_EDGE('',*,*,#8962,.T.);
#12220=ORIENTED_EDGE('',*,*,#8963,.T.);
#12221=ORIENTED_EDGE('',*,*,#8964,.T.);
#12222=ORIENTED_EDGE('',*,*,#8965,.T.);
#12223=ORIENTED_EDGE('',*,*,#8966,.T.);
#12224=ORIENTED_EDGE('',*,*,#8967,.T.);
#12225=ORIENTED_EDGE('',*,*,#8968,.T.);
#12226=ORIENTED_EDGE('',*,*,#8881,.T.);
#12227=ORIENTED_EDGE('',*,*,#8885,.T.);
#12228=ORIENTED_EDGE('',*,*,#8888,.T.);
#12229=ORIENTED_EDGE('',*,*,#8969,.T.);
#12230=ORIENTED_EDGE('',*,*,#8882,.T.);
#12231=ORIENTED_EDGE('',*,*,#8969,.F.);
#12232=ORIENTED_EDGE('',*,*,#8887,.T.);
#12233=ORIENTED_EDGE('',*,*,#8970,.F.);
#12234=ORIENTED_EDGE('',*,*,#8971,.F.);
#12235=ORIENTED_EDGE('',*,*,#8972,.T.);
#12236=ORIENTED_EDGE('',*,*,#8973,.F.);
#12237=ORIENTED_EDGE('',*,*,#8972,.F.);
#12238=ORIENTED_EDGE('',*,*,#8971,.T.);
#12239=ORIENTED_EDGE('',*,*,#8879,.T.);
#12240=ORIENTED_EDGE('',*,*,#8970,.T.);
#12241=ORIENTED_EDGE('',*,*,#8886,.T.);
#12242=ORIENTED_EDGE('',*,*,#8883,.T.);
#12243=ORIENTED_EDGE('',*,*,#8974,.F.);
#12244=ORIENTED_EDGE('',*,*,#8975,.F.);
#12245=ORIENTED_EDGE('',*,*,#8976,.F.);
#12246=ORIENTED_EDGE('',*,*,#8966,.F.);
#12247=ORIENTED_EDGE('',*,*,#8976,.T.);
#12248=ORIENTED_EDGE('',*,*,#8977,.F.);
#12249=ORIENTED_EDGE('',*,*,#8978,.F.);
#12250=ORIENTED_EDGE('',*,*,#8967,.F.);
#12251=ORIENTED_EDGE('',*,*,#8978,.T.);
#12252=ORIENTED_EDGE('',*,*,#8979,.F.);
#12253=ORIENTED_EDGE('',*,*,#8980,.F.);
#12254=ORIENTED_EDGE('',*,*,#8968,.F.);
#12255=ORIENTED_EDGE('',*,*,#8980,.T.);
#12256=ORIENTED_EDGE('',*,*,#8981,.F.);
#12257=ORIENTED_EDGE('',*,*,#8982,.T.);
#12258=ORIENTED_EDGE('',*,*,#8889,.F.);
#12259=ORIENTED_EDGE('',*,*,#8982,.F.);
#12260=ORIENTED_EDGE('',*,*,#8983,.F.);
#12261=ORIENTED_EDGE('',*,*,#8984,.F.);
#12262=ORIENTED_EDGE('',*,*,#8890,.F.);
#12263=ORIENTED_EDGE('',*,*,#8984,.T.);
#12264=ORIENTED_EDGE('',*,*,#8985,.F.);
#12265=ORIENTED_EDGE('',*,*,#8986,.F.);
#12266=ORIENTED_EDGE('',*,*,#8891,.F.);
#12267=ORIENTED_EDGE('',*,*,#8986,.T.);
#12268=ORIENTED_EDGE('',*,*,#8987,.F.);
#12269=ORIENTED_EDGE('',*,*,#8988,.F.);
#12270=ORIENTED_EDGE('',*,*,#8892,.F.);
#12271=ORIENTED_EDGE('',*,*,#8988,.T.);
#12272=ORIENTED_EDGE('',*,*,#8989,.F.);
#12273=ORIENTED_EDGE('',*,*,#8990,.T.);
#12274=ORIENTED_EDGE('',*,*,#8893,.F.);
#12275=ORIENTED_EDGE('',*,*,#8990,.F.);
#12276=ORIENTED_EDGE('',*,*,#8991,.F.);
#12277=ORIENTED_EDGE('',*,*,#8992,.F.);
#12278=ORIENTED_EDGE('',*,*,#8894,.F.);
#12279=ORIENTED_EDGE('',*,*,#8992,.T.);
#12280=ORIENTED_EDGE('',*,*,#8993,.F.);
#12281=ORIENTED_EDGE('',*,*,#8994,.F.);
#12282=ORIENTED_EDGE('',*,*,#8895,.F.);
#12283=ORIENTED_EDGE('',*,*,#8994,.T.);
#12284=ORIENTED_EDGE('',*,*,#8995,.F.);
#12285=ORIENTED_EDGE('',*,*,#8996,.F.);
#12286=ORIENTED_EDGE('',*,*,#8896,.F.);
#12287=ORIENTED_EDGE('',*,*,#8996,.T.);
#12288=ORIENTED_EDGE('',*,*,#8997,.F.);
#12289=ORIENTED_EDGE('',*,*,#8998,.T.);
#12290=ORIENTED_EDGE('',*,*,#8897,.F.);
#12291=ORIENTED_EDGE('',*,*,#8998,.F.);
#12292=ORIENTED_EDGE('',*,*,#8999,.F.);
#12293=ORIENTED_EDGE('',*,*,#9000,.F.);
#12294=ORIENTED_EDGE('',*,*,#8898,.F.);
#12295=ORIENTED_EDGE('',*,*,#9000,.T.);
#12296=ORIENTED_EDGE('',*,*,#9001,.F.);
#12297=ORIENTED_EDGE('',*,*,#9002,.F.);
#12298=ORIENTED_EDGE('',*,*,#8899,.F.);
#12299=ORIENTED_EDGE('',*,*,#9002,.T.);
#12300=ORIENTED_EDGE('',*,*,#9003,.F.);
#12301=ORIENTED_EDGE('',*,*,#9004,.F.);
#12302=ORIENTED_EDGE('',*,*,#8900,.F.);
#12303=ORIENTED_EDGE('',*,*,#9004,.T.);
#12304=ORIENTED_EDGE('',*,*,#9005,.F.);
#12305=ORIENTED_EDGE('',*,*,#9006,.T.);
#12306=ORIENTED_EDGE('',*,*,#8901,.F.);
#12307=ORIENTED_EDGE('',*,*,#9006,.F.);
#12308=ORIENTED_EDGE('',*,*,#9007,.F.);
#12309=ORIENTED_EDGE('',*,*,#9008,.F.);
#12310=ORIENTED_EDGE('',*,*,#8902,.F.);
#12311=ORIENTED_EDGE('',*,*,#9008,.T.);
#12312=ORIENTED_EDGE('',*,*,#9009,.F.);
#12313=ORIENTED_EDGE('',*,*,#9010,.F.);
#12314=ORIENTED_EDGE('',*,*,#8903,.F.);
#12315=ORIENTED_EDGE('',*,*,#9010,.T.);
#12316=ORIENTED_EDGE('',*,*,#9011,.F.);
#12317=ORIENTED_EDGE('',*,*,#9012,.F.);
#12318=ORIENTED_EDGE('',*,*,#8904,.F.);
#12319=ORIENTED_EDGE('',*,*,#9012,.T.);
#12320=ORIENTED_EDGE('',*,*,#9013,.F.);
#12321=ORIENTED_EDGE('',*,*,#9014,.T.);
#12322=ORIENTED_EDGE('',*,*,#8905,.F.);
#12323=ORIENTED_EDGE('',*,*,#9014,.F.);
#12324=ORIENTED_EDGE('',*,*,#9015,.F.);
#12325=ORIENTED_EDGE('',*,*,#9016,.F.);
#12326=ORIENTED_EDGE('',*,*,#8906,.F.);
#12327=ORIENTED_EDGE('',*,*,#9016,.T.);
#12328=ORIENTED_EDGE('',*,*,#9017,.F.);
#12329=ORIENTED_EDGE('',*,*,#9018,.F.);
#12330=ORIENTED_EDGE('',*,*,#8907,.F.);
#12331=ORIENTED_EDGE('',*,*,#9018,.T.);
#12332=ORIENTED_EDGE('',*,*,#9019,.F.);
#12333=ORIENTED_EDGE('',*,*,#9020,.F.);
#12334=ORIENTED_EDGE('',*,*,#8908,.F.);
#12335=ORIENTED_EDGE('',*,*,#9020,.T.);
#12336=ORIENTED_EDGE('',*,*,#9021,.F.);
#12337=ORIENTED_EDGE('',*,*,#9022,.T.);
#12338=ORIENTED_EDGE('',*,*,#8909,.F.);
#12339=ORIENTED_EDGE('',*,*,#9022,.F.);
#12340=ORIENTED_EDGE('',*,*,#9023,.F.);
#12341=ORIENTED_EDGE('',*,*,#9024,.F.);
#12342=ORIENTED_EDGE('',*,*,#8910,.F.);
#12343=ORIENTED_EDGE('',*,*,#9024,.T.);
#12344=ORIENTED_EDGE('',*,*,#9025,.F.);
#12345=ORIENTED_EDGE('',*,*,#9026,.F.);
#12346=ORIENTED_EDGE('',*,*,#8911,.F.);
#12347=ORIENTED_EDGE('',*,*,#9026,.T.);
#12348=ORIENTED_EDGE('',*,*,#9027,.F.);
#12349=ORIENTED_EDGE('',*,*,#9028,.F.);
#12350=ORIENTED_EDGE('',*,*,#8912,.F.);
#12351=ORIENTED_EDGE('',*,*,#9028,.T.);
#12352=ORIENTED_EDGE('',*,*,#9029,.F.);
#12353=ORIENTED_EDGE('',*,*,#9030,.T.);
#12354=ORIENTED_EDGE('',*,*,#8913,.F.);
#12355=ORIENTED_EDGE('',*,*,#9030,.F.);
#12356=ORIENTED_EDGE('',*,*,#9031,.F.);
#12357=ORIENTED_EDGE('',*,*,#9032,.F.);
#12358=ORIENTED_EDGE('',*,*,#8914,.F.);
#12359=ORIENTED_EDGE('',*,*,#9032,.T.);
#12360=ORIENTED_EDGE('',*,*,#9033,.F.);
#12361=ORIENTED_EDGE('',*,*,#9034,.F.);
#12362=ORIENTED_EDGE('',*,*,#8915,.F.);
#12363=ORIENTED_EDGE('',*,*,#9034,.T.);
#12364=ORIENTED_EDGE('',*,*,#9035,.F.);
#12365=ORIENTED_EDGE('',*,*,#9036,.F.);
#12366=ORIENTED_EDGE('',*,*,#8916,.F.);
#12367=ORIENTED_EDGE('',*,*,#9036,.T.);
#12368=ORIENTED_EDGE('',*,*,#9037,.F.);
#12369=ORIENTED_EDGE('',*,*,#9038,.T.);
#12370=ORIENTED_EDGE('',*,*,#8917,.F.);
#12371=ORIENTED_EDGE('',*,*,#9038,.F.);
#12372=ORIENTED_EDGE('',*,*,#9039,.F.);
#12373=ORIENTED_EDGE('',*,*,#9040,.F.);
#12374=ORIENTED_EDGE('',*,*,#8918,.F.);
#12375=ORIENTED_EDGE('',*,*,#9040,.T.);
#12376=ORIENTED_EDGE('',*,*,#9041,.F.);
#12377=ORIENTED_EDGE('',*,*,#9042,.F.);
#12378=ORIENTED_EDGE('',*,*,#8919,.F.);
#12379=ORIENTED_EDGE('',*,*,#9042,.T.);
#12380=ORIENTED_EDGE('',*,*,#9043,.F.);
#12381=ORIENTED_EDGE('',*,*,#9044,.F.);
#12382=ORIENTED_EDGE('',*,*,#8920,.F.);
#12383=ORIENTED_EDGE('',*,*,#9044,.T.);
#12384=ORIENTED_EDGE('',*,*,#9045,.F.);
#12385=ORIENTED_EDGE('',*,*,#9046,.T.);
#12386=ORIENTED_EDGE('',*,*,#8921,.F.);
#12387=ORIENTED_EDGE('',*,*,#9046,.F.);
#12388=ORIENTED_EDGE('',*,*,#9047,.F.);
#12389=ORIENTED_EDGE('',*,*,#9048,.F.);
#12390=ORIENTED_EDGE('',*,*,#8922,.F.);
#12391=ORIENTED_EDGE('',*,*,#9048,.T.);
#12392=ORIENTED_EDGE('',*,*,#9049,.F.);
#12393=ORIENTED_EDGE('',*,*,#9050,.F.);
#12394=ORIENTED_EDGE('',*,*,#8923,.F.);
#12395=ORIENTED_EDGE('',*,*,#9050,.T.);
#12396=ORIENTED_EDGE('',*,*,#9051,.F.);
#12397=ORIENTED_EDGE('',*,*,#9052,.F.);
#12398=ORIENTED_EDGE('',*,*,#8924,.F.);
#12399=ORIENTED_EDGE('',*,*,#9052,.T.);
#12400=ORIENTED_EDGE('',*,*,#9053,.F.);
#12401=ORIENTED_EDGE('',*,*,#9054,.T.);
#12402=ORIENTED_EDGE('',*,*,#8925,.F.);
#12403=ORIENTED_EDGE('',*,*,#9054,.F.);
#12404=ORIENTED_EDGE('',*,*,#9055,.F.);
#12405=ORIENTED_EDGE('',*,*,#9056,.F.);
#12406=ORIENTED_EDGE('',*,*,#8926,.F.);
#12407=ORIENTED_EDGE('',*,*,#9056,.T.);
#12408=ORIENTED_EDGE('',*,*,#9057,.F.);
#12409=ORIENTED_EDGE('',*,*,#9058,.F.);
#12410=ORIENTED_EDGE('',*,*,#8927,.F.);
#12411=ORIENTED_EDGE('',*,*,#9058,.T.);
#12412=ORIENTED_EDGE('',*,*,#9059,.F.);
#12413=ORIENTED_EDGE('',*,*,#9060,.F.);
#12414=ORIENTED_EDGE('',*,*,#8928,.F.);
#12415=ORIENTED_EDGE('',*,*,#9060,.T.);
#12416=ORIENTED_EDGE('',*,*,#9061,.F.);
#12417=ORIENTED_EDGE('',*,*,#9062,.T.);
#12418=ORIENTED_EDGE('',*,*,#8929,.F.);
#12419=ORIENTED_EDGE('',*,*,#9062,.F.);
#12420=ORIENTED_EDGE('',*,*,#9063,.F.);
#12421=ORIENTED_EDGE('',*,*,#9064,.F.);
#12422=ORIENTED_EDGE('',*,*,#8930,.F.);
#12423=ORIENTED_EDGE('',*,*,#9064,.T.);
#12424=ORIENTED_EDGE('',*,*,#9065,.F.);
#12425=ORIENTED_EDGE('',*,*,#9066,.F.);
#12426=ORIENTED_EDGE('',*,*,#8931,.F.);
#12427=ORIENTED_EDGE('',*,*,#9066,.T.);
#12428=ORIENTED_EDGE('',*,*,#9067,.F.);
#12429=ORIENTED_EDGE('',*,*,#9068,.F.);
#12430=ORIENTED_EDGE('',*,*,#8932,.F.);
#12431=ORIENTED_EDGE('',*,*,#9068,.T.);
#12432=ORIENTED_EDGE('',*,*,#9069,.F.);
#12433=ORIENTED_EDGE('',*,*,#9070,.T.);
#12434=ORIENTED_EDGE('',*,*,#8933,.F.);
#12435=ORIENTED_EDGE('',*,*,#9070,.F.);
#12436=ORIENTED_EDGE('',*,*,#9071,.F.);
#12437=ORIENTED_EDGE('',*,*,#9072,.F.);
#12438=ORIENTED_EDGE('',*,*,#8934,.F.);
#12439=ORIENTED_EDGE('',*,*,#9072,.T.);
#12440=ORIENTED_EDGE('',*,*,#9073,.F.);
#12441=ORIENTED_EDGE('',*,*,#9074,.F.);
#12442=ORIENTED_EDGE('',*,*,#8935,.F.);
#12443=ORIENTED_EDGE('',*,*,#9074,.T.);
#12444=ORIENTED_EDGE('',*,*,#9075,.F.);
#12445=ORIENTED_EDGE('',*,*,#9076,.F.);
#12446=ORIENTED_EDGE('',*,*,#8936,.F.);
#12447=ORIENTED_EDGE('',*,*,#9076,.T.);
#12448=ORIENTED_EDGE('',*,*,#9077,.F.);
#12449=ORIENTED_EDGE('',*,*,#9078,.T.);
#12450=ORIENTED_EDGE('',*,*,#8937,.F.);
#12451=ORIENTED_EDGE('',*,*,#9078,.F.);
#12452=ORIENTED_EDGE('',*,*,#9079,.F.);
#12453=ORIENTED_EDGE('',*,*,#9080,.F.);
#12454=ORIENTED_EDGE('',*,*,#8938,.F.);
#12455=ORIENTED_EDGE('',*,*,#9080,.T.);
#12456=ORIENTED_EDGE('',*,*,#9081,.F.);
#12457=ORIENTED_EDGE('',*,*,#9082,.F.);
#12458=ORIENTED_EDGE('',*,*,#8939,.F.);
#12459=ORIENTED_EDGE('',*,*,#9082,.T.);
#12460=ORIENTED_EDGE('',*,*,#9083,.F.);
#12461=ORIENTED_EDGE('',*,*,#9084,.F.);
#12462=ORIENTED_EDGE('',*,*,#8940,.F.);
#12463=ORIENTED_EDGE('',*,*,#9084,.T.);
#12464=ORIENTED_EDGE('',*,*,#9085,.F.);
#12465=ORIENTED_EDGE('',*,*,#9086,.T.);
#12466=ORIENTED_EDGE('',*,*,#8941,.F.);
#12467=ORIENTED_EDGE('',*,*,#9086,.F.);
#12468=ORIENTED_EDGE('',*,*,#9087,.F.);
#12469=ORIENTED_EDGE('',*,*,#9088,.F.);
#12470=ORIENTED_EDGE('',*,*,#8942,.F.);
#12471=ORIENTED_EDGE('',*,*,#9088,.T.);
#12472=ORIENTED_EDGE('',*,*,#9089,.F.);
#12473=ORIENTED_EDGE('',*,*,#9090,.F.);
#12474=ORIENTED_EDGE('',*,*,#8943,.F.);
#12475=ORIENTED_EDGE('',*,*,#9090,.T.);
#12476=ORIENTED_EDGE('',*,*,#9091,.F.);
#12477=ORIENTED_EDGE('',*,*,#9092,.F.);
#12478=ORIENTED_EDGE('',*,*,#8944,.F.);
#12479=ORIENTED_EDGE('',*,*,#9092,.T.);
#12480=ORIENTED_EDGE('',*,*,#9093,.F.);
#12481=ORIENTED_EDGE('',*,*,#9094,.T.);
#12482=ORIENTED_EDGE('',*,*,#8945,.F.);
#12483=ORIENTED_EDGE('',*,*,#9094,.F.);
#12484=ORIENTED_EDGE('',*,*,#9095,.F.);
#12485=ORIENTED_EDGE('',*,*,#9096,.F.);
#12486=ORIENTED_EDGE('',*,*,#8946,.F.);
#12487=ORIENTED_EDGE('',*,*,#9096,.T.);
#12488=ORIENTED_EDGE('',*,*,#9097,.F.);
#12489=ORIENTED_EDGE('',*,*,#9098,.F.);
#12490=ORIENTED_EDGE('',*,*,#8947,.F.);
#12491=ORIENTED_EDGE('',*,*,#9098,.T.);
#12492=ORIENTED_EDGE('',*,*,#9099,.F.);
#12493=ORIENTED_EDGE('',*,*,#9100,.F.);
#12494=ORIENTED_EDGE('',*,*,#8948,.F.);
#12495=ORIENTED_EDGE('',*,*,#9100,.T.);
#12496=ORIENTED_EDGE('',*,*,#9101,.F.);
#12497=ORIENTED_EDGE('',*,*,#9102,.T.);
#12498=ORIENTED_EDGE('',*,*,#8949,.F.);
#12499=ORIENTED_EDGE('',*,*,#9102,.F.);
#12500=ORIENTED_EDGE('',*,*,#9103,.F.);
#12501=ORIENTED_EDGE('',*,*,#9104,.F.);
#12502=ORIENTED_EDGE('',*,*,#8950,.F.);
#12503=ORIENTED_EDGE('',*,*,#9104,.T.);
#12504=ORIENTED_EDGE('',*,*,#9105,.F.);
#12505=ORIENTED_EDGE('',*,*,#9106,.F.);
#12506=ORIENTED_EDGE('',*,*,#8951,.F.);
#12507=ORIENTED_EDGE('',*,*,#9106,.T.);
#12508=ORIENTED_EDGE('',*,*,#9107,.F.);
#12509=ORIENTED_EDGE('',*,*,#9108,.F.);
#12510=ORIENTED_EDGE('',*,*,#8952,.F.);
#12511=ORIENTED_EDGE('',*,*,#9108,.T.);
#12512=ORIENTED_EDGE('',*,*,#9109,.F.);
#12513=ORIENTED_EDGE('',*,*,#9110,.T.);
#12514=ORIENTED_EDGE('',*,*,#8953,.F.);
#12515=ORIENTED_EDGE('',*,*,#9110,.F.);
#12516=ORIENTED_EDGE('',*,*,#9111,.F.);
#12517=ORIENTED_EDGE('',*,*,#9112,.F.);
#12518=ORIENTED_EDGE('',*,*,#8954,.F.);
#12519=ORIENTED_EDGE('',*,*,#9112,.T.);
#12520=ORIENTED_EDGE('',*,*,#9113,.F.);
#12521=ORIENTED_EDGE('',*,*,#9114,.F.);
#12522=ORIENTED_EDGE('',*,*,#8955,.F.);
#12523=ORIENTED_EDGE('',*,*,#9114,.T.);
#12524=ORIENTED_EDGE('',*,*,#9115,.F.);
#12525=ORIENTED_EDGE('',*,*,#9116,.F.);
#12526=ORIENTED_EDGE('',*,*,#8956,.F.);
#12527=ORIENTED_EDGE('',*,*,#9116,.T.);
#12528=ORIENTED_EDGE('',*,*,#9117,.F.);
#12529=ORIENTED_EDGE('',*,*,#9118,.T.);
#12530=ORIENTED_EDGE('',*,*,#8957,.F.);
#12531=ORIENTED_EDGE('',*,*,#9118,.F.);
#12532=ORIENTED_EDGE('',*,*,#9119,.F.);
#12533=ORIENTED_EDGE('',*,*,#9120,.F.);
#12534=ORIENTED_EDGE('',*,*,#8958,.F.);
#12535=ORIENTED_EDGE('',*,*,#9120,.T.);
#12536=ORIENTED_EDGE('',*,*,#9121,.F.);
#12537=ORIENTED_EDGE('',*,*,#9122,.F.);
#12538=ORIENTED_EDGE('',*,*,#8959,.F.);
#12539=ORIENTED_EDGE('',*,*,#9122,.T.);
#12540=ORIENTED_EDGE('',*,*,#9123,.F.);
#12541=ORIENTED_EDGE('',*,*,#9124,.F.);
#12542=ORIENTED_EDGE('',*,*,#8960,.F.);
#12543=ORIENTED_EDGE('',*,*,#9124,.T.);
#12544=ORIENTED_EDGE('',*,*,#9125,.F.);
#12545=ORIENTED_EDGE('',*,*,#9126,.T.);
#12546=ORIENTED_EDGE('',*,*,#8961,.F.);
#12547=ORIENTED_EDGE('',*,*,#9126,.F.);
#12548=ORIENTED_EDGE('',*,*,#9127,.F.);
#12549=ORIENTED_EDGE('',*,*,#9128,.F.);
#12550=ORIENTED_EDGE('',*,*,#8962,.F.);
#12551=ORIENTED_EDGE('',*,*,#9128,.T.);
#12552=ORIENTED_EDGE('',*,*,#9129,.F.);
#12553=ORIENTED_EDGE('',*,*,#9130,.F.);
#12554=ORIENTED_EDGE('',*,*,#8963,.F.);
#12555=ORIENTED_EDGE('',*,*,#9130,.T.);
#12556=ORIENTED_EDGE('',*,*,#9131,.F.);
#12557=ORIENTED_EDGE('',*,*,#9132,.F.);
#12558=ORIENTED_EDGE('',*,*,#8964,.F.);
#12559=ORIENTED_EDGE('',*,*,#9133,.T.);
#12560=ORIENTED_EDGE('',*,*,#9131,.T.);
#12561=ORIENTED_EDGE('',*,*,#9129,.T.);
#12562=ORIENTED_EDGE('',*,*,#9127,.T.);
#12563=ORIENTED_EDGE('',*,*,#9125,.T.);
#12564=ORIENTED_EDGE('',*,*,#9123,.T.);
#12565=ORIENTED_EDGE('',*,*,#9121,.T.);
#12566=ORIENTED_EDGE('',*,*,#9119,.T.);
#12567=ORIENTED_EDGE('',*,*,#9117,.T.);
#12568=ORIENTED_EDGE('',*,*,#9115,.T.);
#12569=ORIENTED_EDGE('',*,*,#9113,.T.);
#12570=ORIENTED_EDGE('',*,*,#9111,.T.);
#12571=ORIENTED_EDGE('',*,*,#9109,.T.);
#12572=ORIENTED_EDGE('',*,*,#9107,.T.);
#12573=ORIENTED_EDGE('',*,*,#9105,.T.);
#12574=ORIENTED_EDGE('',*,*,#9103,.T.);
#12575=ORIENTED_EDGE('',*,*,#9101,.T.);
#12576=ORIENTED_EDGE('',*,*,#9099,.T.);
#12577=ORIENTED_EDGE('',*,*,#9097,.T.);
#12578=ORIENTED_EDGE('',*,*,#9095,.T.);
#12579=ORIENTED_EDGE('',*,*,#9093,.T.);
#12580=ORIENTED_EDGE('',*,*,#9091,.T.);
#12581=ORIENTED_EDGE('',*,*,#9089,.T.);
#12582=ORIENTED_EDGE('',*,*,#9087,.T.);
#12583=ORIENTED_EDGE('',*,*,#9085,.T.);
#12584=ORIENTED_EDGE('',*,*,#9083,.T.);
#12585=ORIENTED_EDGE('',*,*,#9081,.T.);
#12586=ORIENTED_EDGE('',*,*,#9079,.T.);
#12587=ORIENTED_EDGE('',*,*,#9077,.T.);
#12588=ORIENTED_EDGE('',*,*,#9075,.T.);
#12589=ORIENTED_EDGE('',*,*,#9073,.T.);
#12590=ORIENTED_EDGE('',*,*,#9071,.T.);
#12591=ORIENTED_EDGE('',*,*,#9069,.T.);
#12592=ORIENTED_EDGE('',*,*,#9067,.T.);
#12593=ORIENTED_EDGE('',*,*,#9065,.T.);
#12594=ORIENTED_EDGE('',*,*,#9063,.T.);
#12595=ORIENTED_EDGE('',*,*,#9061,.T.);
#12596=ORIENTED_EDGE('',*,*,#9059,.T.);
#12597=ORIENTED_EDGE('',*,*,#9057,.T.);
#12598=ORIENTED_EDGE('',*,*,#9055,.T.);
#12599=ORIENTED_EDGE('',*,*,#9053,.T.);
#12600=ORIENTED_EDGE('',*,*,#9051,.T.);
#12601=ORIENTED_EDGE('',*,*,#9049,.T.);
#12602=ORIENTED_EDGE('',*,*,#9047,.T.);
#12603=ORIENTED_EDGE('',*,*,#9045,.T.);
#12604=ORIENTED_EDGE('',*,*,#9043,.T.);
#12605=ORIENTED_EDGE('',*,*,#9041,.T.);
#12606=ORIENTED_EDGE('',*,*,#9039,.T.);
#12607=ORIENTED_EDGE('',*,*,#9037,.T.);
#12608=ORIENTED_EDGE('',*,*,#9035,.T.);
#12609=ORIENTED_EDGE('',*,*,#9033,.T.);
#12610=ORIENTED_EDGE('',*,*,#9031,.T.);
#12611=ORIENTED_EDGE('',*,*,#9029,.T.);
#12612=ORIENTED_EDGE('',*,*,#9027,.T.);
#12613=ORIENTED_EDGE('',*,*,#9025,.T.);
#12614=ORIENTED_EDGE('',*,*,#9023,.T.);
#12615=ORIENTED_EDGE('',*,*,#9021,.T.);
#12616=ORIENTED_EDGE('',*,*,#9019,.T.);
#12617=ORIENTED_EDGE('',*,*,#9017,.T.);
#12618=ORIENTED_EDGE('',*,*,#9015,.T.);
#12619=ORIENTED_EDGE('',*,*,#9013,.T.);
#12620=ORIENTED_EDGE('',*,*,#9011,.T.);
#12621=ORIENTED_EDGE('',*,*,#9009,.T.);
#12622=ORIENTED_EDGE('',*,*,#9007,.T.);
#12623=ORIENTED_EDGE('',*,*,#9005,.T.);
#12624=ORIENTED_EDGE('',*,*,#9003,.T.);
#12625=ORIENTED_EDGE('',*,*,#9001,.T.);
#12626=ORIENTED_EDGE('',*,*,#8999,.T.);
#12627=ORIENTED_EDGE('',*,*,#8997,.T.);
#12628=ORIENTED_EDGE('',*,*,#8995,.T.);
#12629=ORIENTED_EDGE('',*,*,#8993,.T.);
#12630=ORIENTED_EDGE('',*,*,#8991,.T.);
#12631=ORIENTED_EDGE('',*,*,#8989,.T.);
#12632=ORIENTED_EDGE('',*,*,#8987,.T.);
#12633=ORIENTED_EDGE('',*,*,#8985,.T.);
#12634=ORIENTED_EDGE('',*,*,#8983,.T.);
#12635=ORIENTED_EDGE('',*,*,#8981,.T.);
#12636=ORIENTED_EDGE('',*,*,#8979,.T.);
#12637=ORIENTED_EDGE('',*,*,#8977,.T.);
#12638=ORIENTED_EDGE('',*,*,#8975,.T.);
#12639=ORIENTED_EDGE('',*,*,#8973,.T.);
#12640=ORIENTED_EDGE('',*,*,#8974,.T.);
#12641=ORIENTED_EDGE('',*,*,#8965,.F.);
#12642=ORIENTED_EDGE('',*,*,#9132,.T.);
#12643=ORIENTED_EDGE('',*,*,#9133,.F.);
#12644=ORIENTED_EDGE('',*,*,#9134,.F.);
#12645=ORIENTED_EDGE('',*,*,#9135,.F.);
#12646=ORIENTED_EDGE('',*,*,#9136,.T.);
#12647=ORIENTED_EDGE('',*,*,#9134,.T.);
#12648=ORIENTED_EDGE('',*,*,#9136,.F.);
#12649=ORIENTED_EDGE('',*,*,#9137,.F.);
#12650=ORIENTED_EDGE('',*,*,#9138,.T.);
#12651=ORIENTED_EDGE('',*,*,#9135,.T.);
#12652=ORIENTED_EDGE('',*,*,#9138,.F.);
#12653=ORIENTED_EDGE('',*,*,#9139,.F.);
#12654=ORIENTED_EDGE('',*,*,#9140,.T.);
#12655=ORIENTED_EDGE('',*,*,#9137,.T.);
#12656=ORIENTED_EDGE('',*,*,#9140,.F.);
#12657=ORIENTED_EDGE('',*,*,#9139,.T.);
#12658=ORIENTED_EDGE('',*,*,#9141,.F.);
#12659=ORIENTED_EDGE('',*,*,#9142,.F.);
#12660=ORIENTED_EDGE('',*,*,#9143,.T.);
#12661=ORIENTED_EDGE('',*,*,#9141,.T.);
#12662=ORIENTED_EDGE('',*,*,#9143,.F.);
#12663=ORIENTED_EDGE('',*,*,#9144,.F.);
#12664=ORIENTED_EDGE('',*,*,#9145,.T.);
#12665=ORIENTED_EDGE('',*,*,#9142,.T.);
#12666=ORIENTED_EDGE('',*,*,#9145,.F.);
#12667=ORIENTED_EDGE('',*,*,#9146,.F.);
#12668=ORIENTED_EDGE('',*,*,#9147,.T.);
#12669=ORIENTED_EDGE('',*,*,#9144,.T.);
#12670=ORIENTED_EDGE('',*,*,#9147,.F.);
#12671=ORIENTED_EDGE('',*,*,#9146,.T.);
#12672=ORIENTED_EDGE('',*,*,#9148,.T.);
#12673=ORIENTED_EDGE('',*,*,#9149,.T.);
#12674=ORIENTED_EDGE('',*,*,#9150,.T.);
#12675=ORIENTED_EDGE('',*,*,#9151,.F.);
#12676=ORIENTED_EDGE('',*,*,#9152,.T.);
#12677=ORIENTED_EDGE('',*,*,#9153,.T.);
#12678=ORIENTED_EDGE('',*,*,#9154,.T.);
#12679=ORIENTED_EDGE('',*,*,#9149,.F.);
#12680=ORIENTED_EDGE('',*,*,#9155,.T.);
#12681=ORIENTED_EDGE('',*,*,#9156,.T.);
#12682=ORIENTED_EDGE('',*,*,#9157,.T.);
#12683=ORIENTED_EDGE('',*,*,#9153,.F.);
#12684=ORIENTED_EDGE('',*,*,#9158,.T.);
#12685=ORIENTED_EDGE('',*,*,#9159,.T.);
#12686=ORIENTED_EDGE('',*,*,#9160,.T.);
#12687=ORIENTED_EDGE('',*,*,#9156,.F.);
#12688=ORIENTED_EDGE('',*,*,#9161,.T.);
#12689=ORIENTED_EDGE('',*,*,#9162,.T.);
#12690=ORIENTED_EDGE('',*,*,#9163,.T.);
#12691=ORIENTED_EDGE('',*,*,#9159,.F.);
#12692=ORIENTED_EDGE('',*,*,#9164,.T.);
#12693=ORIENTED_EDGE('',*,*,#9151,.T.);
#12694=ORIENTED_EDGE('',*,*,#9165,.T.);
#12695=ORIENTED_EDGE('',*,*,#9162,.F.);
#12696=ORIENTED_EDGE('',*,*,#9164,.F.);
#12697=ORIENTED_EDGE('',*,*,#9161,.F.);
#12698=ORIENTED_EDGE('',*,*,#9158,.F.);
#12699=ORIENTED_EDGE('',*,*,#9155,.F.);
#12700=ORIENTED_EDGE('',*,*,#9152,.F.);
#12701=ORIENTED_EDGE('',*,*,#9148,.F.);
#12702=ORIENTED_EDGE('',*,*,#9165,.F.);
#12703=ORIENTED_EDGE('',*,*,#9150,.F.);
#12704=ORIENTED_EDGE('',*,*,#9154,.F.);
#12705=ORIENTED_EDGE('',*,*,#9157,.F.);
#12706=ORIENTED_EDGE('',*,*,#9160,.F.);
#12707=ORIENTED_EDGE('',*,*,#9163,.F.);
#12708=ORIENTED_EDGE('',*,*,#9166,.F.);
#12709=ORIENTED_EDGE('',*,*,#9167,.F.);
#12710=ORIENTED_EDGE('',*,*,#9168,.F.);
#12711=ORIENTED_EDGE('',*,*,#9169,.F.);
#12712=ORIENTED_EDGE('',*,*,#9170,.F.);
#12713=ORIENTED_EDGE('',*,*,#9171,.F.);
#12714=ORIENTED_EDGE('',*,*,#9172,.F.);
#12715=ORIENTED_EDGE('',*,*,#9173,.F.);
#12716=ORIENTED_EDGE('',*,*,#9170,.T.);
#12717=ORIENTED_EDGE('',*,*,#9174,.T.);
#12718=ORIENTED_EDGE('',*,*,#9175,.T.);
#12719=ORIENTED_EDGE('',*,*,#9176,.T.);
#12720=ORIENTED_EDGE('',*,*,#9169,.T.);
#12721=ORIENTED_EDGE('',*,*,#9177,.F.);
#12722=ORIENTED_EDGE('',*,*,#9178,.T.);
#12723=ORIENTED_EDGE('',*,*,#9174,.F.);
#12724=ORIENTED_EDGE('',*,*,#9168,.T.);
#12725=ORIENTED_EDGE('',*,*,#9179,.T.);
#12726=ORIENTED_EDGE('',*,*,#9180,.T.);
#12727=ORIENTED_EDGE('',*,*,#9177,.T.);
#12728=ORIENTED_EDGE('',*,*,#9167,.T.);
#12729=ORIENTED_EDGE('',*,*,#9181,.F.);
#12730=ORIENTED_EDGE('',*,*,#9182,.T.);
#12731=ORIENTED_EDGE('',*,*,#9179,.F.);
#12732=ORIENTED_EDGE('',*,*,#9175,.F.);
#12733=ORIENTED_EDGE('',*,*,#9178,.F.);
#12734=ORIENTED_EDGE('',*,*,#9180,.F.);
#12735=ORIENTED_EDGE('',*,*,#9182,.F.);
#12736=ORIENTED_EDGE('',*,*,#9183,.F.);
#12737=ORIENTED_EDGE('',*,*,#9184,.F.);
#12738=ORIENTED_EDGE('',*,*,#9185,.F.);
#12739=ORIENTED_EDGE('',*,*,#9186,.F.);
#12740=ORIENTED_EDGE('',*,*,#9166,.T.);
#12741=ORIENTED_EDGE('',*,*,#9187,.T.);
#12742=ORIENTED_EDGE('',*,*,#9183,.T.);
#12743=ORIENTED_EDGE('',*,*,#9181,.T.);
#12744=ORIENTED_EDGE('',*,*,#9173,.T.);
#12745=ORIENTED_EDGE('',*,*,#9188,.F.);
#12746=ORIENTED_EDGE('',*,*,#9184,.T.);
#12747=ORIENTED_EDGE('',*,*,#9187,.F.);
#12748=ORIENTED_EDGE('',*,*,#9172,.T.);
#12749=ORIENTED_EDGE('',*,*,#9189,.T.);
#12750=ORIENTED_EDGE('',*,*,#9185,.T.);
#12751=ORIENTED_EDGE('',*,*,#9188,.T.);
#12752=ORIENTED_EDGE('',*,*,#9171,.T.);
#12753=ORIENTED_EDGE('',*,*,#9176,.F.);
#12754=ORIENTED_EDGE('',*,*,#9186,.T.);
#12755=ORIENTED_EDGE('',*,*,#9189,.F.);
#12756=ORIENTED_EDGE('',*,*,#9190,.F.);
#12757=ORIENTED_EDGE('',*,*,#9191,.T.);
#12758=ORIENTED_EDGE('',*,*,#9192,.T.);
#12759=ORIENTED_EDGE('',*,*,#9191,.F.);
#12760=ORIENTED_EDGE('',*,*,#9193,.F.);
#12761=ORIENTED_EDGE('',*,*,#9194,.T.);
#12762=ORIENTED_EDGE('',*,*,#9195,.T.);
#12763=ORIENTED_EDGE('',*,*,#9194,.F.);
#12764=ORIENTED_EDGE('',*,*,#9193,.T.);
#12765=ORIENTED_EDGE('',*,*,#9190,.T.);
#12766=ORIENTED_EDGE('',*,*,#9195,.F.);
#12767=ORIENTED_EDGE('',*,*,#9192,.F.);
#12768=ORIENTED_EDGE('',*,*,#9196,.F.);
#12769=ORIENTED_EDGE('',*,*,#9197,.F.);
#12770=ORIENTED_EDGE('',*,*,#9198,.T.);
#12771=ORIENTED_EDGE('',*,*,#9196,.T.);
#12772=ORIENTED_EDGE('',*,*,#9198,.F.);
#12773=ORIENTED_EDGE('',*,*,#9199,.F.);
#12774=ORIENTED_EDGE('',*,*,#9200,.T.);
#12775=ORIENTED_EDGE('',*,*,#9197,.T.);
#12776=ORIENTED_EDGE('',*,*,#9200,.F.);
#12777=ORIENTED_EDGE('',*,*,#9201,.F.);
#12778=ORIENTED_EDGE('',*,*,#9202,.T.);
#12779=ORIENTED_EDGE('',*,*,#9199,.T.);
#12780=ORIENTED_EDGE('',*,*,#9202,.F.);
#12781=ORIENTED_EDGE('',*,*,#9201,.T.);
#12782=ORIENTED_EDGE('',*,*,#9203,.F.);
#12783=ORIENTED_EDGE('',*,*,#9204,.F.);
#12784=ORIENTED_EDGE('',*,*,#9205,.T.);
#12785=ORIENTED_EDGE('',*,*,#9203,.T.);
#12786=ORIENTED_EDGE('',*,*,#9205,.F.);
#12787=ORIENTED_EDGE('',*,*,#9206,.F.);
#12788=ORIENTED_EDGE('',*,*,#9207,.T.);
#12789=ORIENTED_EDGE('',*,*,#9204,.T.);
#12790=ORIENTED_EDGE('',*,*,#9207,.F.);
#12791=ORIENTED_EDGE('',*,*,#9208,.F.);
#12792=ORIENTED_EDGE('',*,*,#9209,.T.);
#12793=ORIENTED_EDGE('',*,*,#9206,.T.);
#12794=ORIENTED_EDGE('',*,*,#9209,.F.);
#12795=ORIENTED_EDGE('',*,*,#9208,.T.);
#12796=ORIENTED_EDGE('',*,*,#9210,.T.);
#12797=ORIENTED_EDGE('',*,*,#9211,.T.);
#12798=ORIENTED_EDGE('',*,*,#9212,.T.);
#12799=ORIENTED_EDGE('',*,*,#9213,.F.);
#12800=ORIENTED_EDGE('',*,*,#9214,.T.);
#12801=ORIENTED_EDGE('',*,*,#9215,.T.);
#12802=ORIENTED_EDGE('',*,*,#9216,.T.);
#12803=ORIENTED_EDGE('',*,*,#9211,.F.);
#12804=ORIENTED_EDGE('',*,*,#9217,.T.);
#12805=ORIENTED_EDGE('',*,*,#9218,.T.);
#12806=ORIENTED_EDGE('',*,*,#9219,.T.);
#12807=ORIENTED_EDGE('',*,*,#9215,.F.);
#12808=ORIENTED_EDGE('',*,*,#9220,.T.);
#12809=ORIENTED_EDGE('',*,*,#9221,.T.);
#12810=ORIENTED_EDGE('',*,*,#9222,.T.);
#12811=ORIENTED_EDGE('',*,*,#9218,.F.);
#12812=ORIENTED_EDGE('',*,*,#9223,.T.);
#12813=ORIENTED_EDGE('',*,*,#9224,.T.);
#12814=ORIENTED_EDGE('',*,*,#9225,.T.);
#12815=ORIENTED_EDGE('',*,*,#9221,.F.);
#12816=ORIENTED_EDGE('',*,*,#9226,.T.);
#12817=ORIENTED_EDGE('',*,*,#9213,.T.);
#12818=ORIENTED_EDGE('',*,*,#9227,.T.);
#12819=ORIENTED_EDGE('',*,*,#9224,.F.);
#12820=ORIENTED_EDGE('',*,*,#9226,.F.);
#12821=ORIENTED_EDGE('',*,*,#9223,.F.);
#12822=ORIENTED_EDGE('',*,*,#9220,.F.);
#12823=ORIENTED_EDGE('',*,*,#9217,.F.);
#12824=ORIENTED_EDGE('',*,*,#9214,.F.);
#12825=ORIENTED_EDGE('',*,*,#9210,.F.);
#12826=ORIENTED_EDGE('',*,*,#9227,.F.);
#12827=ORIENTED_EDGE('',*,*,#9212,.F.);
#12828=ORIENTED_EDGE('',*,*,#9216,.F.);
#12829=ORIENTED_EDGE('',*,*,#9219,.F.);
#12830=ORIENTED_EDGE('',*,*,#9222,.F.);
#12831=ORIENTED_EDGE('',*,*,#9225,.F.);
#12832=ORIENTED_EDGE('',*,*,#9228,.F.);
#12833=ORIENTED_EDGE('',*,*,#9229,.T.);
#12834=ORIENTED_EDGE('',*,*,#9230,.T.);
#12835=ORIENTED_EDGE('',*,*,#9229,.F.);
#12836=ORIENTED_EDGE('',*,*,#9231,.F.);
#12837=ORIENTED_EDGE('',*,*,#9232,.T.);
#12838=ORIENTED_EDGE('',*,*,#9233,.T.);
#12839=ORIENTED_EDGE('',*,*,#9232,.F.);
#12840=ORIENTED_EDGE('',*,*,#9231,.T.);
#12841=ORIENTED_EDGE('',*,*,#9228,.T.);
#12842=ORIENTED_EDGE('',*,*,#9233,.F.);
#12843=ORIENTED_EDGE('',*,*,#9230,.F.);
#12844=CYLINDRICAL_SURFACE('',#14320,0.274999999999999);
#12845=CYLINDRICAL_SURFACE('',#14323,0.274999999999999);
#12846=CYLINDRICAL_SURFACE('',#14326,0.275);
#12847=CYLINDRICAL_SURFACE('',#14329,0.275);
#12848=CYLINDRICAL_SURFACE('',#14353,0.164999999999999);
#12849=CYLINDRICAL_SURFACE('',#14356,0.164999999999999);
#12850=CYLINDRICAL_SURFACE('',#14359,0.164999999999999);
#12851=CYLINDRICAL_SURFACE('',#14362,0.164999999999999);
#12852=CYLINDRICAL_SURFACE('',#14365,0.210000000000001);
#12853=CYLINDRICAL_SURFACE('',#14368,0.210000000000001);
#12854=CYLINDRICAL_SURFACE('',#14371,0.21);
#12855=CYLINDRICAL_SURFACE('',#14374,0.21);
#12856=CYLINDRICAL_SURFACE('',#14377,0.164999999999999);
#12857=CYLINDRICAL_SURFACE('',#14380,0.164999999999999);
#12858=CYLINDRICAL_SURFACE('',#14383,0.165);
#12859=CYLINDRICAL_SURFACE('',#14386,0.164999999999999);
#12860=CYLINDRICAL_SURFACE('',#14389,0.274999999999999);
#12861=CYLINDRICAL_SURFACE('',#14392,0.274999999999999);
#12862=CYLINDRICAL_SURFACE('',#14395,0.275);
#12863=CYLINDRICAL_SURFACE('',#14398,0.275);
#12864=CYLINDRICAL_SURFACE('',#14408,0.5);
#12865=CYLINDRICAL_SURFACE('',#14413,0.5);
#12866=CYLINDRICAL_SURFACE('',#14418,0.275);
#12867=CYLINDRICAL_SURFACE('',#14420,0.275);
#12868=CYLINDRICAL_SURFACE('',#14436,0.5);
#12869=CYLINDRICAL_SURFACE('',#14441,0.5);
#12870=CYLINDRICAL_SURFACE('',#14446,0.274999999999999);
#12871=CYLINDRICAL_SURFACE('',#14448,0.274999999999999);
#12872=CYLINDRICAL_SURFACE('',#14464,0.225);
#12873=CYLINDRICAL_SURFACE('',#14467,0.225);
#12874=CYLINDRICAL_SURFACE('',#14470,0.164999999999999);
#12875=CYLINDRICAL_SURFACE('',#14473,0.164999999999999);
#12876=CYLINDRICAL_SURFACE('',#14476,0.164999999999999);
#12877=CYLINDRICAL_SURFACE('',#14479,0.164999999999999);
#12878=CYLINDRICAL_SURFACE('',#14482,1.6);
#12879=CYLINDRICAL_SURFACE('',#14496,0.225);
#12880=CYLINDRICAL_SURFACE('',#14499,0.225);
#12881=CYLINDRICAL_SURFACE('',#14502,0.225);
#12882=CYLINDRICAL_SURFACE('',#14505,0.225);
#12883=CYLINDRICAL_SURFACE('',#14508,1.59);
#12884=CYLINDRICAL_SURFACE('',#14513,1.2);
#12885=CYLINDRICAL_SURFACE('',#14515,2.4);
#12886=CYLINDRICAL_SURFACE('',#14521,0.225);
#12887=CYLINDRICAL_SURFACE('',#14524,0.225);
#12888=CYLINDRICAL_SURFACE('',#14527,0.225);
#12889=CYLINDRICAL_SURFACE('',#14530,0.225);
#12890=CYLINDRICAL_SURFACE('',#14533,1.59);
#12891=CYLINDRICAL_SURFACE('',#14538,1.2);
#12892=CYLINDRICAL_SURFACE('',#14540,2.4);
#12893=CYLINDRICAL_SURFACE('',#14546,0.225);
#12894=CYLINDRICAL_SURFACE('',#14549,0.225);
#12895=CYLINDRICAL_SURFACE('',#14552,0.164999999999999);
#12896=CYLINDRICAL_SURFACE('',#14555,0.164999999999999);
#12897=CYLINDRICAL_SURFACE('',#14558,0.164999999999999);
#12898=CYLINDRICAL_SURFACE('',#14561,0.164999999999999);
#12899=CYLINDRICAL_SURFACE('',#14564,1.6);
#12900=CYLINDRICAL_SURFACE('',#14578,0.225);
#12901=CYLINDRICAL_SURFACE('',#14581,0.225);
#12902=CYLINDRICAL_SURFACE('',#14584,0.225);
#12903=CYLINDRICAL_SURFACE('',#14587,0.225);
#12904=CYLINDRICAL_SURFACE('',#14590,1.59);
#12905=CYLINDRICAL_SURFACE('',#14595,1.2);
#12906=CYLINDRICAL_SURFACE('',#14597,2.4);
#12907=CYLINDRICAL_SURFACE('',#14603,0.225);
#12908=CYLINDRICAL_SURFACE('',#14606,0.225);
#12909=CYLINDRICAL_SURFACE('',#14609,0.225);
#12910=CYLINDRICAL_SURFACE('',#14612,0.225);
#12911=CYLINDRICAL_SURFACE('',#14615,1.59);
#12912=CYLINDRICAL_SURFACE('',#14620,1.2);
#12913=CYLINDRICAL_SURFACE('',#14622,2.4);
#12914=CYLINDRICAL_SURFACE('',#14664,0.21);
#12915=CYLINDRICAL_SURFACE('',#14689,0.2117);
#12916=CYLINDRICAL_SURFACE('',#14702,0.265);
#12917=CYLINDRICAL_SURFACE('',#14706,0.5);
#12918=CYLINDRICAL_SURFACE('',#14710,0.375);
#12919=CYLINDRICAL_SURFACE('',#14715,0.375);
#12920=CYLINDRICAL_SURFACE('',#14720,0.375);
#12921=CYLINDRICAL_SURFACE('',#14725,0.375);
#12922=CYLINDRICAL_SURFACE('',#14730,0.225);
#12923=CYLINDRICAL_SURFACE('',#14732,0.225);
#12924=CYLINDRICAL_SURFACE('',#14734,0.225);
#12925=CYLINDRICAL_SURFACE('',#14736,0.225000000000001);
#12926=CYLINDRICAL_SURFACE('',#14757,0.425);
#12927=CYLINDRICAL_SURFACE('',#14765,0.24505);
#12928=CYLINDRICAL_SURFACE('',#14786,1.070235);
#12929=CYLINDRICAL_SURFACE('',#14788,0.6);
#12930=CYLINDRICAL_SURFACE('',#14794,1.070235);
#12931=CYLINDRICAL_SURFACE('',#14806,1.129765);
#12932=CYLINDRICAL_SURFACE('',#14813,1.6);
#12933=CYLINDRICAL_SURFACE('',#14818,1.129765);
#12934=CYLINDRICAL_SURFACE('',#14838,1.123812);
#12935=CYLINDRICAL_SURFACE('',#14874,1.076188);
#12936=CYLINDRICAL_SURFACE('',#14888,1.119765);
#12937=CYLINDRICAL_SURFACE('',#14892,1.085235);
#12938=CYLINDRICAL_SURFACE('',#14896,1.119765);
#12939=CYLINDRICAL_SURFACE('',#14900,1.085235);
#12940=CYLINDRICAL_SURFACE('',#14921,0.35);
#12941=CYLINDRICAL_SURFACE('',#14929,0.1954);
#12942=CYLINDRICAL_SURFACE('',#14932,0.225000000000001);
#12943=CYLINDRICAL_SURFACE('',#14935,0.225);
#12944=CYLINDRICAL_SURFACE('',#14938,0.225);
#12945=CYLINDRICAL_SURFACE('',#14941,0.225000000000001);
#12946=CYLINDRICAL_SURFACE('',#14944,0.275);
#12947=CYLINDRICAL_SURFACE('',#14947,0.275);
#12948=CYLINDRICAL_SURFACE('',#14950,0.275);
#12949=CYLINDRICAL_SURFACE('',#14953,0.275);
#12950=CYLINDRICAL_SURFACE('',#14963,0.164999999999999);
#12951=CYLINDRICAL_SURFACE('',#14967,0.165);
#12952=CYLINDRICAL_SURFACE('',#14971,0.165);
#12953=CYLINDRICAL_SURFACE('',#14975,0.164999999999999);
#12954=CYLINDRICAL_SURFACE('',#15113,0.21);
#12955=CYLINDRICAL_SURFACE('',#15119,0.21);
#12956=CYLINDRICAL_SURFACE('',#15125,0.21);
#12957=CYLINDRICAL_SURFACE('',#15131,0.21);
#12958=CYLINDRICAL_SURFACE('',#15189,0.425);
#12959=CYLINDRICAL_SURFACE('',#15197,0.24505);
#12960=CYLINDRICAL_SURFACE('',#15207,0.164999999999999);
#12961=CYLINDRICAL_SURFACE('',#15211,0.164999999999999);
#12962=CYLINDRICAL_SURFACE('',#15228,0.800000000000001);
#12963=CYLINDRICAL_SURFACE('',#15229,0.6);
#12964=CYLINDRICAL_SURFACE('',#15231,0.6);
#12965=CYLINDRICAL_SURFACE('',#15236,0.605);
#12966=CYLINDRICAL_SURFACE('',#15239,0.800000000000001);
#12967=CYLINDRICAL_SURFACE('',#15245,0.605);
#12968=CYLINDRICAL_SURFACE('',#15248,0.800000000000001);
#12969=CYLINDRICAL_SURFACE('',#15254,0.605);
#12970=CYLINDRICAL_SURFACE('',#15257,0.800000000000001);
#12971=CYLINDRICAL_SURFACE('',#15263,0.225);
#12972=CYLINDRICAL_SURFACE('',#15266,1.);
#12973=CYLINDRICAL_SURFACE('',#15272,0.225);
#12974=CYLINDRICAL_SURFACE('',#15275,1.);
#12975=CYLINDRICAL_SURFACE('',#15281,0.605);
#12976=CYLINDRICAL_SURFACE('',#15284,0.800000000000001);
#12977=CYLINDRICAL_SURFACE('',#15290,0.25);
#12978=CYLINDRICAL_SURFACE('',#15299,0.6);
#12979=CYLINDRICAL_SURFACE('',#15301,0.9);
#12980=CYLINDRICAL_SURFACE('',#15310,1.2);
#12981=CYLINDRICAL_SURFACE('',#15314,0.33);
#12982=CYLINDRICAL_SURFACE('',#15317,0.4);
#12983=CYLINDRICAL_SURFACE('',#15348,0.6);
#12984=CYLINDRICAL_SURFACE('',#15350,1.4);
#12985=CYLINDRICAL_SURFACE('',#15355,1.75);
#12986=CYLINDRICAL_SURFACE('',#15358,1.75);
#12987=CYLINDRICAL_SURFACE('',#15361,1.75);
#12988=CYLINDRICAL_SURFACE('',#15364,1.75);
#12989=CYLINDRICAL_SURFACE('',#15367,1.75);
#12990=CYLINDRICAL_SURFACE('',#15370,1.75);
#12991=CYLINDRICAL_SURFACE('',#15373,1.75);
#12992=CYLINDRICAL_SURFACE('',#15376,1.75);
#12993=CYLINDRICAL_SURFACE('',#15379,1.75);
#12994=CYLINDRICAL_SURFACE('',#15382,1.75);
#12995=CYLINDRICAL_SURFACE('',#15385,1.75);
#12996=CYLINDRICAL_SURFACE('',#15388,1.75);
#12997=CYLINDRICAL_SURFACE('',#15391,1.75);
#12998=CYLINDRICAL_SURFACE('',#15394,1.75);
#12999=CYLINDRICAL_SURFACE('',#15397,1.75);
#13000=CYLINDRICAL_SURFACE('',#15400,1.75);
#13001=CYLINDRICAL_SURFACE('',#15403,1.75);
#13002=CYLINDRICAL_SURFACE('',#15406,1.75);
#13003=CYLINDRICAL_SURFACE('',#15409,1.75);
#13004=CYLINDRICAL_SURFACE('',#15414,1.75);
#13005=CYLINDRICAL_SURFACE('',#15420,0.35);
#13006=CYLINDRICAL_SURFACE('',#15428,0.1954);
#13007=CYLINDRICAL_SURFACE('',#15535,0.32);
#13008=CYLINDRICAL_SURFACE('',#15538,0.6);
#13009=CYLINDRICAL_SURFACE('',#15548,0.5);
#13010=CYLINDRICAL_SURFACE('',#15556,0.2942);
#13011=CYLINDRICAL_SURFACE('',#15587,0.404999999999999);
#13012=CYLINDRICAL_SURFACE('',#15590,0.9);
#13013=ADVANCED_FACE('',(#1535),#12844,.F.);
#13014=ADVANCED_FACE('',(#1536),#12845,.F.);
#13015=ADVANCED_FACE('',(#1537),#12846,.F.);
#13016=ADVANCED_FACE('',(#1538),#12847,.F.);
#13017=ADVANCED_FACE('',(#1539),#1044,.T.);
#13018=ADVANCED_FACE('',(#1540),#1045,.T.);
#13019=ADVANCED_FACE('',(#1541),#1046,.T.);
#13020=ADVANCED_FACE('',(#1542),#1047,.T.);
#13021=ADVANCED_FACE('',(#1543,#833,#834,#835,#836),#1048,.T.);
#13022=ADVANCED_FACE('',(#1544,#837,#838,#839,#840),#1049,.F.);
#13023=ADVANCED_FACE('',(#1545),#1050,.T.);
#13024=ADVANCED_FACE('',(#1546),#1051,.T.);
#13025=ADVANCED_FACE('',(#1547),#1052,.T.);
#13026=ADVANCED_FACE('',(#1548),#1053,.T.);
#13027=ADVANCED_FACE('',(#1549),#1054,.T.);
#13028=ADVANCED_FACE('',(#1550),#1055,.F.);
#13029=ADVANCED_FACE('',(#1551),#1056,.T.);
#13030=ADVANCED_FACE('',(#1552),#1057,.T.);
#13031=ADVANCED_FACE('',(#1553),#1058,.T.);
#13032=ADVANCED_FACE('',(#1554),#1059,.T.);
#13033=ADVANCED_FACE('',(#1555),#1060,.T.);
#13034=ADVANCED_FACE('',(#1556),#1061,.F.);
#13035=ADVANCED_FACE('',(#1557),#12848,.F.);
#13036=ADVANCED_FACE('',(#1558),#12849,.F.);
#13037=ADVANCED_FACE('',(#1559),#12850,.F.);
#13038=ADVANCED_FACE('',(#1560),#12851,.F.);
#13039=ADVANCED_FACE('',(#1561),#12852,.F.);
#13040=ADVANCED_FACE('',(#1562),#12853,.F.);
#13041=ADVANCED_FACE('',(#1563),#12854,.F.);
#13042=ADVANCED_FACE('',(#1564),#12855,.F.);
#13043=ADVANCED_FACE('',(#1565),#12856,.F.);
#13044=ADVANCED_FACE('',(#1566),#12857,.F.);
#13045=ADVANCED_FACE('',(#1567),#12858,.F.);
#13046=ADVANCED_FACE('',(#1568),#12859,.F.);
#13047=ADVANCED_FACE('',(#1569),#12860,.F.);
#13048=ADVANCED_FACE('',(#1570),#12861,.F.);
#13049=ADVANCED_FACE('',(#1571),#12862,.F.);
#13050=ADVANCED_FACE('',(#1572),#12863,.F.);
#13051=ADVANCED_FACE('',(#1573),#1062,.T.);
#13052=ADVANCED_FACE('',(#1574),#1063,.T.);
#13053=ADVANCED_FACE('',(#1575),#1064,.T.);
#13054=ADVANCED_FACE('',(#1576),#1065,.T.);
#13055=ADVANCED_FACE('',(#1577,#841,#842,#843,#844,#845,#846,#847,#848,
#849,#850,#851,#852,#853,#854,#855,#856),#1066,.T.);
#13056=ADVANCED_FACE('',(#1578,#857,#858,#859,#860,#861,#862,#863,#864,
#865,#866,#867,#868,#869,#870,#871,#872),#1067,.F.);
#13057=ADVANCED_FACE('',(#1579),#12864,.F.);
#13058=ADVANCED_FACE('',(#1580,#873),#1068,.T.);
#13059=ADVANCED_FACE('',(#1581),#12865,.F.);
#13060=ADVANCED_FACE('',(#1582,#874),#1069,.T.);
#13061=ADVANCED_FACE('',(#1583),#12866,.F.);
#13062=ADVANCED_FACE('',(#1584),#12867,.F.);
#13063=ADVANCED_FACE('',(#1585),#1070,.T.);
#13064=ADVANCED_FACE('',(#1586),#1071,.T.);
#13065=ADVANCED_FACE('',(#1587),#1072,.T.);
#13066=ADVANCED_FACE('',(#1588),#1073,.T.);
#13067=ADVANCED_FACE('',(#1589,#875,#876),#1074,.T.);
#13068=ADVANCED_FACE('',(#1590,#877,#878),#1075,.F.);
#13069=ADVANCED_FACE('',(#1591),#1076,.T.);
#13070=ADVANCED_FACE('',(#1592),#1077,.T.);
#13071=ADVANCED_FACE('',(#1593),#1078,.T.);
#13072=ADVANCED_FACE('',(#1594),#1079,.T.);
#13073=ADVANCED_FACE('',(#1595),#1080,.T.);
#13074=ADVANCED_FACE('',(#1596),#1081,.F.);
#13075=ADVANCED_FACE('',(#1597),#12868,.F.);
#13076=ADVANCED_FACE('',(#1598,#879),#1082,.T.);
#13077=ADVANCED_FACE('',(#1599),#12869,.F.);
#13078=ADVANCED_FACE('',(#1600,#880),#1083,.T.);
#13079=ADVANCED_FACE('',(#1601),#12870,.F.);
#13080=ADVANCED_FACE('',(#1602),#12871,.F.);
#13081=ADVANCED_FACE('',(#1603),#1084,.T.);
#13082=ADVANCED_FACE('',(#1604),#1085,.T.);
#13083=ADVANCED_FACE('',(#1605),#1086,.T.);
#13084=ADVANCED_FACE('',(#1606),#1087,.T.);
#13085=ADVANCED_FACE('',(#1607,#881,#882),#1088,.T.);
#13086=ADVANCED_FACE('',(#1608,#883,#884),#1089,.F.);
#13087=ADVANCED_FACE('',(#1609),#1090,.T.);
#13088=ADVANCED_FACE('',(#1610),#1091,.T.);
#13089=ADVANCED_FACE('',(#1611),#1092,.T.);
#13090=ADVANCED_FACE('',(#1612),#1093,.T.);
#13091=ADVANCED_FACE('',(#1613),#1094,.T.);
#13092=ADVANCED_FACE('',(#1614),#1095,.F.);
#13093=ADVANCED_FACE('',(#1615),#12872,.F.);
#13094=ADVANCED_FACE('',(#1616),#12873,.F.);
#13095=ADVANCED_FACE('',(#1617),#12874,.F.);
#13096=ADVANCED_FACE('',(#1618),#12875,.F.);
#13097=ADVANCED_FACE('',(#1619),#12876,.F.);
#13098=ADVANCED_FACE('',(#1620),#12877,.F.);
#13099=ADVANCED_FACE('',(#1621),#12878,.F.);
#13100=ADVANCED_FACE('',(#1622,#885),#1096,.T.);
#13101=ADVANCED_FACE('',(#1623,#886),#1097,.T.);
#13102=ADVANCED_FACE('',(#1624),#1098,.T.);
#13103=ADVANCED_FACE('',(#1625),#1099,.T.);
#13104=ADVANCED_FACE('',(#1626,#887,#888,#889,#890,#891),#1100,.T.);
#13105=ADVANCED_FACE('',(#1627),#1101,.T.);
#13106=ADVANCED_FACE('',(#1628,#892,#893,#894,#895,#896),#1102,.T.);
#13107=ADVANCED_FACE('',(#1629),#1103,.T.);
#13108=ADVANCED_FACE('',(#1630),#1104,.T.);
#13109=ADVANCED_FACE('',(#1631,#897,#898),#1105,.F.);
#13110=ADVANCED_FACE('',(#1632),#12879,.F.);
#13111=ADVANCED_FACE('',(#1633),#12880,.F.);
#13112=ADVANCED_FACE('',(#1634),#12881,.F.);
#13113=ADVANCED_FACE('',(#1635),#12882,.F.);
#13114=ADVANCED_FACE('',(#1636),#12883,.T.);
#13115=ADVANCED_FACE('',(#1637,#899),#1106,.T.);
#13116=ADVANCED_FACE('',(#1638),#12884,.F.);
#13117=ADVANCED_FACE('',(#1639),#12885,.T.);
#13118=ADVANCED_FACE('',(#1640,#900,#901,#902,#903,#904),#1107,.T.);
#13119=ADVANCED_FACE('',(#1641,#905,#906,#907,#908,#909),#1108,.F.);
#13120=ADVANCED_FACE('',(#1642),#12886,.F.);
#13121=ADVANCED_FACE('',(#1643),#12887,.F.);
#13122=ADVANCED_FACE('',(#1644),#12888,.F.);
#13123=ADVANCED_FACE('',(#1645),#12889,.F.);
#13124=ADVANCED_FACE('',(#1646),#12890,.T.);
#13125=ADVANCED_FACE('',(#1647,#910),#1109,.F.);
#13126=ADVANCED_FACE('',(#1648),#12891,.F.);
#13127=ADVANCED_FACE('',(#1649),#12892,.T.);
#13128=ADVANCED_FACE('',(#1650,#911,#912,#913,#914,#915),#1110,.T.);
#13129=ADVANCED_FACE('',(#1651,#916,#917,#918,#919,#920),#1111,.F.);
#13130=ADVANCED_FACE('',(#1652),#12893,.F.);
#13131=ADVANCED_FACE('',(#1653),#12894,.F.);
#13132=ADVANCED_FACE('',(#1654),#12895,.F.);
#13133=ADVANCED_FACE('',(#1655),#12896,.F.);
#13134=ADVANCED_FACE('',(#1656),#12897,.F.);
#13135=ADVANCED_FACE('',(#1657),#12898,.F.);
#13136=ADVANCED_FACE('',(#1658),#12899,.F.);
#13137=ADVANCED_FACE('',(#1659,#921),#1112,.T.);
#13138=ADVANCED_FACE('',(#1660,#922),#1113,.T.);
#13139=ADVANCED_FACE('',(#1661),#1114,.T.);
#13140=ADVANCED_FACE('',(#1662),#1115,.T.);
#13141=ADVANCED_FACE('',(#1663,#923,#924,#925,#926,#927),#1116,.T.);
#13142=ADVANCED_FACE('',(#1664),#1117,.T.);
#13143=ADVANCED_FACE('',(#1665,#928,#929,#930,#931,#932),#1118,.T.);
#13144=ADVANCED_FACE('',(#1666),#1119,.T.);
#13145=ADVANCED_FACE('',(#1667),#1120,.T.);
#13146=ADVANCED_FACE('',(#1668,#933,#934),#1121,.F.);
#13147=ADVANCED_FACE('',(#1669),#12900,.F.);
#13148=ADVANCED_FACE('',(#1670),#12901,.F.);
#13149=ADVANCED_FACE('',(#1671),#12902,.F.);
#13150=ADVANCED_FACE('',(#1672),#12903,.F.);
#13151=ADVANCED_FACE('',(#1673),#12904,.T.);
#13152=ADVANCED_FACE('',(#1674,#935),#1122,.T.);
#13153=ADVANCED_FACE('',(#1675),#12905,.F.);
#13154=ADVANCED_FACE('',(#1676),#12906,.T.);
#13155=ADVANCED_FACE('',(#1677,#936,#937,#938,#939,#940),#1123,.T.);
#13156=ADVANCED_FACE('',(#1678,#941,#942,#943,#944,#945),#1124,.F.);
#13157=ADVANCED_FACE('',(#1679),#12907,.F.);
#13158=ADVANCED_FACE('',(#1680),#12908,.F.);
#13159=ADVANCED_FACE('',(#1681),#12909,.F.);
#13160=ADVANCED_FACE('',(#1682),#12910,.F.);
#13161=ADVANCED_FACE('',(#1683),#12911,.T.);
#13162=ADVANCED_FACE('',(#1684,#946),#1125,.F.);
#13163=ADVANCED_FACE('',(#1685),#12912,.F.);
#13164=ADVANCED_FACE('',(#1686),#12913,.T.);
#13165=ADVANCED_FACE('',(#1687,#947,#948,#949,#950,#951),#1126,.T.);
#13166=ADVANCED_FACE('',(#1688,#952,#953,#954,#955,#956),#1127,.F.);
#13167=ADVANCED_FACE('',(#1689),#1128,.F.);
#13168=ADVANCED_FACE('',(#1690),#1129,.F.);
#13169=ADVANCED_FACE('',(#1691),#1130,.F.);
#13170=ADVANCED_FACE('',(#1692),#1131,.F.);
#13171=ADVANCED_FACE('',(#1693),#1132,.F.);
#13172=ADVANCED_FACE('',(#1694),#1133,.F.);
#13173=ADVANCED_FACE('',(#1695),#1134,.F.);
#13174=ADVANCED_FACE('',(#1696),#1135,.F.);
#13175=ADVANCED_FACE('',(#1697),#1136,.F.);
#13176=ADVANCED_FACE('',(#1698),#1137,.F.);
#13177=ADVANCED_FACE('',(#1699),#1138,.F.);
#13178=ADVANCED_FACE('',(#1700),#1139,.F.);
#13179=ADVANCED_FACE('',(#1701),#1140,.F.);
#13180=ADVANCED_FACE('',(#1702),#1141,.F.);
#13181=ADVANCED_FACE('',(#1703),#1142,.F.);
#13182=ADVANCED_FACE('',(#1704),#1143,.F.);
#13183=ADVANCED_FACE('',(#1705),#1144,.F.);
#13184=ADVANCED_FACE('',(#1706),#1145,.F.);
#13185=ADVANCED_FACE('',(#1707),#1146,.F.);
#13186=ADVANCED_FACE('',(#1708),#1147,.F.);
#13187=ADVANCED_FACE('',(#1709),#1148,.F.);
#13188=ADVANCED_FACE('',(#1710),#1149,.F.);
#13189=ADVANCED_FACE('',(#1711),#1150,.F.);
#13190=ADVANCED_FACE('',(#1712),#1151,.F.);
#13191=ADVANCED_FACE('',(#1713),#1152,.F.);
#13192=ADVANCED_FACE('',(#1714),#1153,.F.);
#13193=ADVANCED_FACE('',(#1715),#1154,.F.);
#13194=ADVANCED_FACE('',(#1716),#1155,.F.);
#13195=ADVANCED_FACE('',(#1717),#1156,.F.);
#13196=ADVANCED_FACE('',(#1718),#1157,.F.);
#13197=ADVANCED_FACE('',(#1719),#1158,.F.);
#13198=ADVANCED_FACE('',(#1720),#1159,.F.);
#13199=ADVANCED_FACE('',(#1721),#1160,.F.);
#13200=ADVANCED_FACE('',(#1722),#1161,.F.);
#13201=ADVANCED_FACE('',(#1723),#1162,.F.);
#13202=ADVANCED_FACE('',(#1724),#1163,.F.);
#13203=ADVANCED_FACE('',(#1725),#12914,.F.);
#13204=ADVANCED_FACE('',(#1726),#1164,.T.);
#13205=ADVANCED_FACE('',(#1727),#1165,.T.);
#13206=ADVANCED_FACE('',(#1728),#1166,.T.);
#13207=ADVANCED_FACE('',(#1729),#1167,.T.);
#13208=ADVANCED_FACE('',(#1730),#1168,.T.);
#13209=ADVANCED_FACE('',(#1731),#1169,.T.);
#13210=ADVANCED_FACE('',(#1732),#1170,.T.);
#13211=ADVANCED_FACE('',(#1733),#1171,.T.);
#13212=ADVANCED_FACE('',(#1734,#957),#1172,.T.);
#13213=ADVANCED_FACE('',(#1735,#958),#1173,.F.);
#13214=ADVANCED_FACE('',(#1736),#1174,.F.);
#13215=ADVANCED_FACE('',(#1737),#1175,.T.);
#13216=ADVANCED_FACE('',(#1738,#959),#1176,.T.);
#13217=ADVANCED_FACE('',(#1739),#1177,.T.);
#13218=ADVANCED_FACE('',(#1740),#1178,.T.);
#13219=ADVANCED_FACE('',(#1741),#1179,.F.);
#13220=ADVANCED_FACE('',(#1742),#1180,.T.);
#13221=ADVANCED_FACE('',(#1743),#1181,.T.);
#13222=ADVANCED_FACE('',(#1744),#1182,.T.);
#13223=ADVANCED_FACE('',(#1745),#12915,.F.);
#13224=ADVANCED_FACE('',(#1746),#1183,.F.);
#13225=ADVANCED_FACE('',(#1747),#1184,.F.);
#13226=ADVANCED_FACE('',(#1748),#1185,.T.);
#13227=ADVANCED_FACE('',(#1749),#1186,.T.);
#13228=ADVANCED_FACE('',(#1750),#615,.F.);
#13229=ADVANCED_FACE('',(#1751),#12916,.F.);
#13230=ADVANCED_FACE('',(#1752,#960),#1187,.T.);
#13231=ADVANCED_FACE('',(#1753),#12917,.T.);
#13232=ADVANCED_FACE('',(#1754,#961),#1188,.F.);
#13233=ADVANCED_FACE('',(#1755),#12918,.F.);
#13234=ADVANCED_FACE('',(#1756,#962),#1189,.T.);
#13235=ADVANCED_FACE('',(#1757),#12919,.F.);
#13236=ADVANCED_FACE('',(#1758,#963),#1190,.T.);
#13237=ADVANCED_FACE('',(#1759),#12920,.F.);
#13238=ADVANCED_FACE('',(#1760,#964),#1191,.T.);
#13239=ADVANCED_FACE('',(#1761),#12921,.F.);
#13240=ADVANCED_FACE('',(#1762,#965),#1192,.T.);
#13241=ADVANCED_FACE('',(#1763),#12922,.F.);
#13242=ADVANCED_FACE('',(#1764),#12923,.F.);
#13243=ADVANCED_FACE('',(#1765),#12924,.F.);
#13244=ADVANCED_FACE('',(#1766),#12925,.F.);
#13245=ADVANCED_FACE('',(#1767),#1193,.T.);
#13246=ADVANCED_FACE('',(#1768),#1194,.T.);
#13247=ADVANCED_FACE('',(#1769),#1195,.T.);
#13248=ADVANCED_FACE('',(#1770),#1196,.T.);
#13249=ADVANCED_FACE('',(#1771,#966,#967,#968,#969),#1197,.T.);
#13250=ADVANCED_FACE('',(#1772),#1198,.T.);
#13251=ADVANCED_FACE('',(#1773),#1199,.T.);
#13252=ADVANCED_FACE('',(#1774),#1200,.T.);
#13253=ADVANCED_FACE('',(#1775),#1201,.T.);
#13254=ADVANCED_FACE('',(#1776),#1202,.T.);
#13255=ADVANCED_FACE('',(#1777,#970,#971,#972,#973),#1203,.T.);
#13256=ADVANCED_FACE('',(#1778),#1204,.T.);
#13257=ADVANCED_FACE('',(#1779),#1205,.T.);
#13258=ADVANCED_FACE('',(#1780),#1206,.F.);
#13259=ADVANCED_FACE('',(#1781),#1207,.T.);
#13260=ADVANCED_FACE('',(#1782),#616,.T.);
#13261=ADVANCED_FACE('',(#1783),#12926,.T.);
#13262=ADVANCED_FACE('',(#1784),#617,.T.);
#13263=ADVANCED_FACE('',(#1785,#974),#1208,.T.);
#13264=ADVANCED_FACE('',(#1786),#618,.T.);
#13265=ADVANCED_FACE('',(#1787),#12927,.T.);
#13266=ADVANCED_FACE('',(#1788),#619,.T.);
#13267=ADVANCED_FACE('',(#1789),#1209,.T.);
#13268=ADVANCED_FACE('',(#1790),#1210,.F.);
#13269=ADVANCED_FACE('',(#1791),#1211,.F.);
#13270=ADVANCED_FACE('',(#1792),#1212,.F.);
#13271=ADVANCED_FACE('',(#1793),#1213,.F.);
#13272=ADVANCED_FACE('',(#1794),#1214,.F.);
#13273=ADVANCED_FACE('',(#1795),#1215,.F.);
#13274=ADVANCED_FACE('',(#1796),#1216,.F.);
#13275=ADVANCED_FACE('',(#1797),#1217,.F.);
#13276=ADVANCED_FACE('',(#1798),#603,.F.);
#13277=ADVANCED_FACE('',(#1799),#12928,.T.);
#13278=ADVANCED_FACE('',(#1800),#12929,.F.);
#13279=ADVANCED_FACE('',(#1801),#620,.F.);
#13280=ADVANCED_FACE('',(#1802,#975),#1218,.T.);
#13281=ADVANCED_FACE('',(#1803),#12930,.T.);
#13282=ADVANCED_FACE('',(#1804,#976),#1219,.T.);
#13283=ADVANCED_FACE('',(#1805),#621,.F.);
#13284=ADVANCED_FACE('',(#1806),#604,.F.);
#13285=ADVANCED_FACE('',(#1807),#12931,.F.);
#13286=ADVANCED_FACE('',(#1808,#977),#1220,.T.);
#13287=ADVANCED_FACE('',(#1809),#622,.T.);
#13288=ADVANCED_FACE('',(#1810),#12932,.T.);
#13289=ADVANCED_FACE('',(#1811),#623,.T.);
#13290=ADVANCED_FACE('',(#1812,#978),#1221,.T.);
#13291=ADVANCED_FACE('',(#1813),#12933,.F.);
#13292=ADVANCED_FACE('',(#1814),#589,.T.);
#13293=ADVANCED_FACE('',(#1815),#590,.T.);
#13294=ADVANCED_FACE('',(#1816),#591,.T.);
#13295=ADVANCED_FACE('',(#1817),#592,.T.);
#13296=ADVANCED_FACE('',(#1818),#593,.T.);
#13297=ADVANCED_FACE('',(#1819),#594,.T.);
#13298=ADVANCED_FACE('',(#1820),#595,.T.);
#13299=ADVANCED_FACE('',(#1821),#596,.F.);
#13300=ADVANCED_FACE('',(#1822),#12934,.T.);
#13301=ADVANCED_FACE('',(#1823),#1222,.T.);
#13302=ADVANCED_FACE('',(#1824),#597,.F.);
#13303=ADVANCED_FACE('',(#1825),#1223,.T.);
#13304=ADVANCED_FACE('',(#1826),#598,.F.);
#13305=ADVANCED_FACE('',(#1827),#1224,.T.);
#13306=ADVANCED_FACE('',(#1828),#599,.F.);
#13307=ADVANCED_FACE('',(#1829),#1225,.T.);
#13308=ADVANCED_FACE('',(#1830),#600,.F.);
#13309=ADVANCED_FACE('',(#1831),#1226,.T.);
#13310=ADVANCED_FACE('',(#1832),#601,.F.);
#13311=ADVANCED_FACE('',(#1833),#12935,.F.);
#13312=ADVANCED_FACE('',(#1834),#1227,.T.);
#13313=ADVANCED_FACE('',(#1835),#602,.F.);
#13314=ADVANCED_FACE('',(#1836,#979),#1228,.T.);
#13315=ADVANCED_FACE('',(#1837),#1229,.T.);
#13316=ADVANCED_FACE('',(#1838,#980),#1230,.T.);
#13317=ADVANCED_FACE('',(#1839),#12936,.T.);
#13318=ADVANCED_FACE('',(#1840,#981),#1231,.T.);
#13319=ADVANCED_FACE('',(#1841),#12937,.F.);
#13320=ADVANCED_FACE('',(#1842,#982),#1232,.T.);
#13321=ADVANCED_FACE('',(#1843),#12938,.T.);
#13322=ADVANCED_FACE('',(#1844,#983),#1233,.T.);
#13323=ADVANCED_FACE('',(#1845),#12939,.F.);
#13324=ADVANCED_FACE('',(#1846),#1234,.F.);
#13325=ADVANCED_FACE('',(#1847),#1235,.F.);
#13326=ADVANCED_FACE('',(#1848),#1236,.F.);
#13327=ADVANCED_FACE('',(#1849),#1237,.F.);
#13328=ADVANCED_FACE('',(#1850),#1238,.F.);
#13329=ADVANCED_FACE('',(#1851),#1239,.F.);
#13330=ADVANCED_FACE('',(#1852),#1240,.F.);
#13331=ADVANCED_FACE('',(#1853),#1241,.F.);
#13332=ADVANCED_FACE('',(#1854),#1242,.F.);
#13333=ADVANCED_FACE('',(#1855),#1243,.T.);
#13334=ADVANCED_FACE('',(#1856),#624,.T.);
#13335=ADVANCED_FACE('',(#1857),#12940,.T.);
#13336=ADVANCED_FACE('',(#1858),#625,.T.);
#13337=ADVANCED_FACE('',(#1859,#984),#1244,.T.);
#13338=ADVANCED_FACE('',(#1860),#626,.T.);
#13339=ADVANCED_FACE('',(#1861),#12941,.T.);
#13340=ADVANCED_FACE('',(#1862),#12942,.F.);
#13341=ADVANCED_FACE('',(#1863),#12943,.F.);
#13342=ADVANCED_FACE('',(#1864),#12944,.F.);
#13343=ADVANCED_FACE('',(#1865),#12945,.F.);
#13344=ADVANCED_FACE('',(#1866),#12946,.F.);
#13345=ADVANCED_FACE('',(#1867),#12947,.F.);
#13346=ADVANCED_FACE('',(#1868),#12948,.F.);
#13347=ADVANCED_FACE('',(#1869),#12949,.F.);
#13348=ADVANCED_FACE('',(#1870),#1245,.T.);
#13349=ADVANCED_FACE('',(#1871),#1246,.T.);
#13350=ADVANCED_FACE('',(#1872),#1247,.T.);
#13351=ADVANCED_FACE('',(#1873),#1248,.T.);
#13352=ADVANCED_FACE('',(#1874,#985,#986,#987,#988,#989,#990,#991,#992),
#1249,.T.);
#13353=ADVANCED_FACE('',(#1875,#993,#994,#995,#996,#997,#998,#999,#1000),
#1250,.F.);
#13354=ADVANCED_FACE('',(#1876),#12950,.F.);
#13355=ADVANCED_FACE('',(#1877),#1251,.F.);
#13356=ADVANCED_FACE('',(#1878),#12951,.F.);
#13357=ADVANCED_FACE('',(#1879),#1252,.F.);
#13358=ADVANCED_FACE('',(#1880),#12952,.F.);
#13359=ADVANCED_FACE('',(#1881),#1253,.F.);
#13360=ADVANCED_FACE('',(#1882),#12953,.F.);
#13361=ADVANCED_FACE('',(#1883),#1254,.F.);
#13362=ADVANCED_FACE('',(#1884),#1255,.T.);
#13363=ADVANCED_FACE('',(#1885,#1001,#1002,#1003,#1004),#1256,.T.);
#13364=ADVANCED_FACE('',(#1886),#1257,.T.);
#13365=ADVANCED_FACE('',(#1887),#1258,.T.);
#13366=ADVANCED_FACE('',(#1888),#1259,.T.);
#13367=ADVANCED_FACE('',(#1889),#1260,.T.);
#13368=ADVANCED_FACE('',(#1890),#1261,.T.);
#13369=ADVANCED_FACE('',(#1891),#1262,.T.);
#13370=ADVANCED_FACE('',(#1892),#1263,.T.);
#13371=ADVANCED_FACE('',(#1893),#1264,.T.);
#13372=ADVANCED_FACE('',(#1894),#1265,.T.);
#13373=ADVANCED_FACE('',(#1895),#1266,.T.);
#13374=ADVANCED_FACE('',(#1896),#1267,.T.);
#13375=ADVANCED_FACE('',(#1897),#1268,.T.);
#13376=ADVANCED_FACE('',(#1898),#1269,.T.);
#13377=ADVANCED_FACE('',(#1899),#1270,.T.);
#13378=ADVANCED_FACE('',(#1900),#1271,.T.);
#13379=ADVANCED_FACE('',(#1901),#1272,.T.);
#13380=ADVANCED_FACE('',(#1902),#1273,.T.);
#13381=ADVANCED_FACE('',(#1903),#1274,.T.);
#13382=ADVANCED_FACE('',(#1904),#1275,.T.);
#13383=ADVANCED_FACE('',(#1905),#1276,.T.);
#13384=ADVANCED_FACE('',(#1906),#1277,.T.);
#13385=ADVANCED_FACE('',(#1907),#1278,.T.);
#13386=ADVANCED_FACE('',(#1908),#1279,.T.);
#13387=ADVANCED_FACE('',(#1909),#1280,.T.);
#13388=ADVANCED_FACE('',(#1910),#1281,.T.);
#13389=ADVANCED_FACE('',(#1911),#1282,.T.);
#13390=ADVANCED_FACE('',(#1912),#1283,.T.);
#13391=ADVANCED_FACE('',(#1913),#1284,.T.);
#13392=ADVANCED_FACE('',(#1914),#1285,.T.);
#13393=ADVANCED_FACE('',(#1915),#1286,.T.);
#13394=ADVANCED_FACE('',(#1916),#1287,.T.);
#13395=ADVANCED_FACE('',(#1917),#1288,.T.);
#13396=ADVANCED_FACE('',(#1918),#1289,.T.);
#13397=ADVANCED_FACE('',(#1919),#1290,.T.);
#13398=ADVANCED_FACE('',(#1920),#1291,.T.);
#13399=ADVANCED_FACE('',(#1921),#1292,.T.);
#13400=ADVANCED_FACE('',(#1922),#1293,.T.);
#13401=ADVANCED_FACE('',(#1923),#1294,.T.);
#13402=ADVANCED_FACE('',(#1924),#1295,.T.);
#13403=ADVANCED_FACE('',(#1925),#1296,.T.);
#13404=ADVANCED_FACE('',(#1926),#1297,.T.);
#13405=ADVANCED_FACE('',(#1927),#1298,.T.);
#13406=ADVANCED_FACE('',(#1928),#1299,.T.);
#13407=ADVANCED_FACE('',(#1929),#1300,.T.);
#13408=ADVANCED_FACE('',(#1930),#1301,.T.);
#13409=ADVANCED_FACE('',(#1931),#1302,.T.);
#13410=ADVANCED_FACE('',(#1932),#1303,.T.);
#13411=ADVANCED_FACE('',(#1933),#1304,.T.);
#13412=ADVANCED_FACE('',(#1934),#1305,.T.);
#13413=ADVANCED_FACE('',(#1935),#1306,.T.);
#13414=ADVANCED_FACE('',(#1936),#1307,.T.);
#13415=ADVANCED_FACE('',(#1937),#1308,.T.);
#13416=ADVANCED_FACE('',(#1938),#1309,.T.);
#13417=ADVANCED_FACE('',(#1939),#1310,.T.);
#13418=ADVANCED_FACE('',(#1940),#1311,.T.);
#13419=ADVANCED_FACE('',(#1941),#1312,.T.);
#13420=ADVANCED_FACE('',(#1942),#1313,.T.);
#13421=ADVANCED_FACE('',(#1943),#1314,.T.);
#13422=ADVANCED_FACE('',(#1944),#1315,.T.);
#13423=ADVANCED_FACE('',(#1945),#1316,.T.);
#13424=ADVANCED_FACE('',(#1946),#1317,.T.);
#13425=ADVANCED_FACE('',(#1947),#1318,.T.);
#13426=ADVANCED_FACE('',(#1948),#1319,.T.);
#13427=ADVANCED_FACE('',(#1949),#1320,.T.);
#13428=ADVANCED_FACE('',(#1950),#1321,.T.);
#13429=ADVANCED_FACE('',(#1951),#1322,.T.);
#13430=ADVANCED_FACE('',(#1952),#1323,.T.);
#13431=ADVANCED_FACE('',(#1953),#1324,.T.);
#13432=ADVANCED_FACE('',(#1954),#1325,.T.);
#13433=ADVANCED_FACE('',(#1955),#1326,.T.);
#13434=ADVANCED_FACE('',(#1956),#1327,.T.);
#13435=ADVANCED_FACE('',(#1957),#1328,.T.);
#13436=ADVANCED_FACE('',(#1958),#1329,.T.);
#13437=ADVANCED_FACE('',(#1959),#1330,.T.);
#13438=ADVANCED_FACE('',(#1960),#1331,.T.);
#13439=ADVANCED_FACE('',(#1961),#1332,.T.);
#13440=ADVANCED_FACE('',(#1962),#1333,.T.);
#13441=ADVANCED_FACE('',(#1963),#1334,.T.);
#13442=ADVANCED_FACE('',(#1964),#1335,.T.);
#13443=ADVANCED_FACE('',(#1965),#1336,.T.);
#13444=ADVANCED_FACE('',(#1966),#1337,.T.);
#13445=ADVANCED_FACE('',(#1967),#1338,.T.);
#13446=ADVANCED_FACE('',(#1968),#1339,.T.);
#13447=ADVANCED_FACE('',(#1969),#1340,.T.);
#13448=ADVANCED_FACE('',(#1970),#1341,.T.);
#13449=ADVANCED_FACE('',(#1971),#1342,.T.);
#13450=ADVANCED_FACE('',(#1972),#1343,.T.);
#13451=ADVANCED_FACE('',(#1973),#1344,.T.);
#13452=ADVANCED_FACE('',(#1974),#1345,.T.);
#13453=ADVANCED_FACE('',(#1975),#1346,.T.);
#13454=ADVANCED_FACE('',(#1976),#1347,.T.);
#13455=ADVANCED_FACE('',(#1977),#1348,.T.);
#13456=ADVANCED_FACE('',(#1978),#1349,.T.);
#13457=ADVANCED_FACE('',(#1979),#1350,.T.);
#13458=ADVANCED_FACE('',(#1980),#1351,.T.);
#13459=ADVANCED_FACE('',(#1981),#1352,.T.);
#13460=ADVANCED_FACE('',(#1982),#1353,.T.);
#13461=ADVANCED_FACE('',(#1983),#1354,.T.);
#13462=ADVANCED_FACE('',(#1984),#1355,.T.);
#13463=ADVANCED_FACE('',(#1985),#1356,.T.);
#13464=ADVANCED_FACE('',(#1986),#1357,.T.);
#13465=ADVANCED_FACE('',(#1987),#1358,.T.);
#13466=ADVANCED_FACE('',(#1988),#1359,.T.);
#13467=ADVANCED_FACE('',(#1989),#1360,.T.);
#13468=ADVANCED_FACE('',(#1990),#1361,.T.);
#13469=ADVANCED_FACE('',(#1991),#1362,.T.);
#13470=ADVANCED_FACE('',(#1992),#1363,.T.);
#13471=ADVANCED_FACE('',(#1993),#1364,.T.);
#13472=ADVANCED_FACE('',(#1994),#1365,.T.);
#13473=ADVANCED_FACE('',(#1995),#1366,.T.);
#13474=ADVANCED_FACE('',(#1996),#1367,.T.);
#13475=ADVANCED_FACE('',(#1997),#1368,.T.);
#13476=ADVANCED_FACE('',(#1998),#1369,.T.);
#13477=ADVANCED_FACE('',(#1999),#1370,.T.);
#13478=ADVANCED_FACE('',(#2000),#1371,.T.);
#13479=ADVANCED_FACE('',(#2001),#1372,.T.);
#13480=ADVANCED_FACE('',(#2002),#1373,.T.);
#13481=ADVANCED_FACE('',(#2003),#1374,.T.);
#13482=ADVANCED_FACE('',(#2004),#1375,.T.);
#13483=ADVANCED_FACE('',(#2005),#1376,.T.);
#13484=ADVANCED_FACE('',(#2006),#1377,.T.);
#13485=ADVANCED_FACE('',(#2007),#1378,.T.);
#13486=ADVANCED_FACE('',(#2008),#1379,.T.);
#13487=ADVANCED_FACE('',(#2009),#1380,.T.);
#13488=ADVANCED_FACE('',(#2010),#1381,.T.);
#13489=ADVANCED_FACE('',(#2011),#1382,.T.);
#13490=ADVANCED_FACE('',(#2012),#1383,.T.);
#13491=ADVANCED_FACE('',(#2013),#1384,.F.);
#13492=ADVANCED_FACE('',(#2014),#1385,.T.);
#13493=ADVANCED_FACE('',(#2015),#12954,.F.);
#13494=ADVANCED_FACE('',(#2016),#1386,.T.);
#13495=ADVANCED_FACE('',(#2017),#12955,.F.);
#13496=ADVANCED_FACE('',(#2018),#1387,.T.);
#13497=ADVANCED_FACE('',(#2019),#12956,.F.);
#13498=ADVANCED_FACE('',(#2020),#1388,.T.);
#13499=ADVANCED_FACE('',(#2021),#12957,.F.);
#13500=ADVANCED_FACE('',(#2022),#1389,.T.);
#13501=ADVANCED_FACE('',(#2023),#1390,.T.);
#13502=ADVANCED_FACE('',(#2024),#1391,.T.);
#13503=ADVANCED_FACE('',(#2025),#1392,.T.);
#13504=ADVANCED_FACE('',(#2026),#1393,.T.);
#13505=ADVANCED_FACE('',(#2027,#1005,#1006,#1007,#1008),#1394,.T.);
#13506=ADVANCED_FACE('',(#2028),#1395,.T.);
#13507=ADVANCED_FACE('',(#2029),#1396,.T.);
#13508=ADVANCED_FACE('',(#2030),#1397,.T.);
#13509=ADVANCED_FACE('',(#2031),#1398,.T.);
#13510=ADVANCED_FACE('',(#2032),#1399,.T.);
#13511=ADVANCED_FACE('',(#2033),#1400,.T.);
#13512=ADVANCED_FACE('',(#2034),#1401,.T.);
#13513=ADVANCED_FACE('',(#2035),#1402,.T.);
#13514=ADVANCED_FACE('',(#2036),#1403,.T.);
#13515=ADVANCED_FACE('',(#2037),#1404,.T.);
#13516=ADVANCED_FACE('',(#2038),#1405,.T.);
#13517=ADVANCED_FACE('',(#2039),#1406,.T.);
#13518=ADVANCED_FACE('',(#2040),#1407,.T.);
#13519=ADVANCED_FACE('',(#2041),#1408,.T.);
#13520=ADVANCED_FACE('',(#2042),#1409,.T.);
#13521=ADVANCED_FACE('',(#2043),#1410,.T.);
#13522=ADVANCED_FACE('',(#2044),#1411,.T.);
#13523=ADVANCED_FACE('',(#2045),#1412,.F.);
#13524=ADVANCED_FACE('',(#2046),#1413,.T.);
#13525=ADVANCED_FACE('',(#2047),#1414,.T.);
#13526=ADVANCED_FACE('',(#2048),#1415,.T.);
#13527=ADVANCED_FACE('',(#2049),#1416,.T.);
#13528=ADVANCED_FACE('',(#2050),#1417,.T.);
#13529=ADVANCED_FACE('',(#2051),#1418,.T.);
#13530=ADVANCED_FACE('',(#2052),#1419,.T.);
#13531=ADVANCED_FACE('',(#2053),#1420,.T.);
#13532=ADVANCED_FACE('',(#2054),#1421,.T.);
#13533=ADVANCED_FACE('',(#2055),#1422,.T.);
#13534=ADVANCED_FACE('',(#2056),#1423,.F.);
#13535=ADVANCED_FACE('',(#2057),#1424,.F.);
#13536=ADVANCED_FACE('',(#2058),#1425,.F.);
#13537=ADVANCED_FACE('',(#2059),#1426,.F.);
#13538=ADVANCED_FACE('',(#2060),#1427,.F.);
#13539=ADVANCED_FACE('',(#2061),#1428,.F.);
#13540=ADVANCED_FACE('',(#2062),#1429,.F.);
#13541=ADVANCED_FACE('',(#2063),#1430,.F.);
#13542=ADVANCED_FACE('',(#2064),#1431,.F.);
#13543=ADVANCED_FACE('',(#2065),#1432,.T.);
#13544=ADVANCED_FACE('',(#2066),#627,.T.);
#13545=ADVANCED_FACE('',(#2067),#12958,.T.);
#13546=ADVANCED_FACE('',(#2068),#628,.T.);
#13547=ADVANCED_FACE('',(#2069,#1009),#1433,.T.);
#13548=ADVANCED_FACE('',(#2070),#629,.T.);
#13549=ADVANCED_FACE('',(#2071),#12959,.T.);
#13550=ADVANCED_FACE('',(#2072),#1434,.F.);
#13551=ADVANCED_FACE('',(#2073),#1435,.T.);
#13552=ADVANCED_FACE('',(#2074),#1436,.F.);
#13553=ADVANCED_FACE('',(#2075),#1437,.F.);
#13554=ADVANCED_FACE('',(#2076),#1438,.F.);
#13555=ADVANCED_FACE('',(#2077),#12960,.F.);
#13556=ADVANCED_FACE('',(#2078),#1439,.T.);
#13557=ADVANCED_FACE('',(#2079),#12961,.F.);
#13558=ADVANCED_FACE('',(#2080),#1440,.F.);
#13559=ADVANCED_FACE('',(#2081),#1441,.F.);
#13560=ADVANCED_FACE('',(#2082),#1442,.T.);
#13561=ADVANCED_FACE('',(#2083),#1443,.F.);
#13562=ADVANCED_FACE('',(#2084),#1444,.F.);
#13563=ADVANCED_FACE('',(#2085),#1445,.F.);
#13564=ADVANCED_FACE('',(#2086,#1010),#1446,.T.);
#13565=ADVANCED_FACE('',(#2087,#1011),#1447,.F.);
#13566=ADVANCED_FACE('',(#2088),#12962,.T.);
#13567=ADVANCED_FACE('',(#2089),#12963,.T.);
#13568=ADVANCED_FACE('',(#2090,#1012,#1013),#12964,.T.);
#13569=ADVANCED_FACE('',(#2091,#1014),#1448,.T.);
#13570=ADVANCED_FACE('',(#2092,#1015),#1449,.F.);
#13571=ADVANCED_FACE('',(#2093),#12965,.F.);
#13572=ADVANCED_FACE('',(#2094),#12966,.T.);
#13573=ADVANCED_FACE('',(#2095,#1016),#1450,.T.);
#13574=ADVANCED_FACE('',(#2096,#1017),#1451,.F.);
#13575=ADVANCED_FACE('',(#2097),#12967,.F.);
#13576=ADVANCED_FACE('',(#2098),#12968,.T.);
#13577=ADVANCED_FACE('',(#2099,#1018),#1452,.T.);
#13578=ADVANCED_FACE('',(#2100,#1019),#1453,.F.);
#13579=ADVANCED_FACE('',(#2101),#12969,.F.);
#13580=ADVANCED_FACE('',(#2102),#12970,.T.);
#13581=ADVANCED_FACE('',(#2103,#1020),#1454,.T.);
#13582=ADVANCED_FACE('',(#2104,#1021),#1455,.F.);
#13583=ADVANCED_FACE('',(#2105),#12971,.F.);
#13584=ADVANCED_FACE('',(#2106),#12972,.T.);
#13585=ADVANCED_FACE('',(#2107,#1022),#1456,.T.);
#13586=ADVANCED_FACE('',(#2108,#1023),#1457,.F.);
#13587=ADVANCED_FACE('',(#2109),#12973,.F.);
#13588=ADVANCED_FACE('',(#2110),#12974,.T.);
#13589=ADVANCED_FACE('',(#2111,#1024),#1458,.T.);
#13590=ADVANCED_FACE('',(#2112,#1025),#1459,.F.);
#13591=ADVANCED_FACE('',(#2113),#12975,.F.);
#13592=ADVANCED_FACE('',(#2114),#12976,.T.);
#13593=ADVANCED_FACE('',(#2115,#1026),#1460,.T.);
#13594=ADVANCED_FACE('',(#2116,#1027),#1461,.F.);
#13595=ADVANCED_FACE('',(#2117),#12977,.F.);
#13596=ADVANCED_FACE('',(#2118),#1462,.F.);
#13597=ADVANCED_FACE('',(#2119),#1463,.F.);
#13598=ADVANCED_FACE('',(#2120),#1464,.F.);
#13599=ADVANCED_FACE('',(#2121,#1028),#1465,.T.);
#13600=ADVANCED_FACE('',(#2122),#12978,.F.);
#13601=ADVANCED_FACE('',(#2123),#12979,.T.);
#13602=ADVANCED_FACE('',(#2124),#1466,.T.);
#13603=ADVANCED_FACE('',(#2125,#1029),#1467,.F.);
#13604=ADVANCED_FACE('',(#2126),#1468,.T.);
#13605=ADVANCED_FACE('',(#2127,#1030),#1469,.T.);
#13606=ADVANCED_FACE('',(#2128,#1031),#12980,.T.);
#13607=ADVANCED_FACE('',(#2129,#1032),#1470,.F.);
#13608=ADVANCED_FACE('',(#2130),#12981,.F.);
#13609=ADVANCED_FACE('',(#2131),#12982,.T.);
#13610=ADVANCED_FACE('',(#2132,#1033),#1471,.T.);
#13611=ADVANCED_FACE('',(#2133,#1034),#1472,.F.);
#13612=ADVANCED_FACE('',(#2134),#1473,.F.);
#13613=ADVANCED_FACE('',(#2135),#1474,.F.);
#13614=ADVANCED_FACE('',(#2136),#1475,.F.);
#13615=ADVANCED_FACE('',(#2137,#1035),#1476,.F.);
#13616=ADVANCED_FACE('',(#2138),#12983,.F.);
#13617=ADVANCED_FACE('',(#2139),#12984,.T.);
#13618=ADVANCED_FACE('',(#2140,#1036),#1477,.T.);
#13619=ADVANCED_FACE('',(#2141),#11,.T.);
#13620=ADVANCED_FACE('',(#2142),#1478,.T.);
#13621=ADVANCED_FACE('',(#2143),#12,.T.);
#13622=ADVANCED_FACE('',(#2144),#12985,.T.);
#13623=ADVANCED_FACE('',(#2145),#13,.T.);
#13624=ADVANCED_FACE('',(#2146),#1479,.T.);
#13625=ADVANCED_FACE('',(#2147),#14,.T.);
#13626=ADVANCED_FACE('',(#2148),#12986,.T.);
#13627=ADVANCED_FACE('',(#2149),#15,.T.);
#13628=ADVANCED_FACE('',(#2150),#1480,.T.);
#13629=ADVANCED_FACE('',(#2151),#16,.T.);
#13630=ADVANCED_FACE('',(#2152),#12987,.T.);
#13631=ADVANCED_FACE('',(#2153),#17,.T.);
#13632=ADVANCED_FACE('',(#2154),#1481,.T.);
#13633=ADVANCED_FACE('',(#2155),#18,.T.);
#13634=ADVANCED_FACE('',(#2156),#12988,.T.);
#13635=ADVANCED_FACE('',(#2157),#19,.T.);
#13636=ADVANCED_FACE('',(#2158),#1482,.T.);
#13637=ADVANCED_FACE('',(#2159),#20,.T.);
#13638=ADVANCED_FACE('',(#2160),#12989,.T.);
#13639=ADVANCED_FACE('',(#2161),#21,.T.);
#13640=ADVANCED_FACE('',(#2162),#1483,.T.);
#13641=ADVANCED_FACE('',(#2163),#22,.T.);
#13642=ADVANCED_FACE('',(#2164),#12990,.T.);
#13643=ADVANCED_FACE('',(#2165),#23,.T.);
#13644=ADVANCED_FACE('',(#2166),#1484,.T.);
#13645=ADVANCED_FACE('',(#2167),#24,.T.);
#13646=ADVANCED_FACE('',(#2168),#12991,.T.);
#13647=ADVANCED_FACE('',(#2169),#25,.T.);
#13648=ADVANCED_FACE('',(#2170),#1485,.T.);
#13649=ADVANCED_FACE('',(#2171),#26,.T.);
#13650=ADVANCED_FACE('',(#2172),#12992,.T.);
#13651=ADVANCED_FACE('',(#2173),#27,.T.);
#13652=ADVANCED_FACE('',(#2174),#1486,.T.);
#13653=ADVANCED_FACE('',(#2175),#28,.T.);
#13654=ADVANCED_FACE('',(#2176),#12993,.T.);
#13655=ADVANCED_FACE('',(#2177),#29,.T.);
#13656=ADVANCED_FACE('',(#2178),#1487,.T.);
#13657=ADVANCED_FACE('',(#2179),#30,.T.);
#13658=ADVANCED_FACE('',(#2180),#12994,.T.);
#13659=ADVANCED_FACE('',(#2181),#31,.T.);
#13660=ADVANCED_FACE('',(#2182),#1488,.T.);
#13661=ADVANCED_FACE('',(#2183),#32,.T.);
#13662=ADVANCED_FACE('',(#2184),#12995,.T.);
#13663=ADVANCED_FACE('',(#2185),#33,.T.);
#13664=ADVANCED_FACE('',(#2186),#1489,.T.);
#13665=ADVANCED_FACE('',(#2187),#34,.T.);
#13666=ADVANCED_FACE('',(#2188),#12996,.T.);
#13667=ADVANCED_FACE('',(#2189),#35,.T.);
#13668=ADVANCED_FACE('',(#2190),#1490,.T.);
#13669=ADVANCED_FACE('',(#2191),#36,.T.);
#13670=ADVANCED_FACE('',(#2192),#12997,.T.);
#13671=ADVANCED_FACE('',(#2193),#37,.T.);
#13672=ADVANCED_FACE('',(#2194),#1491,.T.);
#13673=ADVANCED_FACE('',(#2195),#38,.T.);
#13674=ADVANCED_FACE('',(#2196),#12998,.T.);
#13675=ADVANCED_FACE('',(#2197),#39,.T.);
#13676=ADVANCED_FACE('',(#2198),#1492,.T.);
#13677=ADVANCED_FACE('',(#2199),#40,.T.);
#13678=ADVANCED_FACE('',(#2200),#12999,.T.);
#13679=ADVANCED_FACE('',(#2201),#41,.T.);
#13680=ADVANCED_FACE('',(#2202),#1493,.T.);
#13681=ADVANCED_FACE('',(#2203),#42,.T.);
#13682=ADVANCED_FACE('',(#2204),#13000,.T.);
#13683=ADVANCED_FACE('',(#2205),#43,.T.);
#13684=ADVANCED_FACE('',(#2206),#1494,.T.);
#13685=ADVANCED_FACE('',(#2207),#44,.T.);
#13686=ADVANCED_FACE('',(#2208),#13001,.T.);
#13687=ADVANCED_FACE('',(#2209),#45,.T.);
#13688=ADVANCED_FACE('',(#2210),#1495,.T.);
#13689=ADVANCED_FACE('',(#2211),#46,.T.);
#13690=ADVANCED_FACE('',(#2212),#13002,.T.);
#13691=ADVANCED_FACE('',(#2213),#47,.T.);
#13692=ADVANCED_FACE('',(#2214),#1496,.T.);
#13693=ADVANCED_FACE('',(#2215),#48,.T.);
#13694=ADVANCED_FACE('',(#2216),#13003,.T.);
#13695=ADVANCED_FACE('',(#2217),#49,.T.);
#13696=ADVANCED_FACE('',(#2218),#1497,.T.);
#13697=ADVANCED_FACE('',(#2219),#50,.T.);
#13698=ADVANCED_FACE('',(#2220,#1037),#1498,.T.);
#13699=ADVANCED_FACE('',(#2221),#13004,.T.);
#13700=ADVANCED_FACE('',(#2222),#1499,.T.);
#13701=ADVANCED_FACE('',(#2223),#630,.T.);
#13702=ADVANCED_FACE('',(#2224),#13005,.T.);
#13703=ADVANCED_FACE('',(#2225),#631,.T.);
#13704=ADVANCED_FACE('',(#2226,#1038),#1500,.T.);
#13705=ADVANCED_FACE('',(#2227),#632,.T.);
#13706=ADVANCED_FACE('',(#2228),#13006,.T.);
#13707=ADVANCED_FACE('',(#2229),#633,.T.);
#13708=ADVANCED_FACE('',(#2230),#1501,.T.);
#13709=ADVANCED_FACE('',(#2231),#1502,.F.);
#13710=ADVANCED_FACE('',(#2232),#1503,.F.);
#13711=ADVANCED_FACE('',(#2233),#1504,.F.);
#13712=ADVANCED_FACE('',(#2234),#1505,.F.);
#13713=ADVANCED_FACE('',(#2235),#1506,.F.);
#13714=ADVANCED_FACE('',(#2236),#1507,.F.);
#13715=ADVANCED_FACE('',(#2237),#1508,.F.);
#13716=ADVANCED_FACE('',(#2238),#1509,.F.);
#13717=ADVANCED_FACE('',(#2239),#1510,.T.);
#13718=ADVANCED_FACE('',(#2240),#1511,.T.);
#13719=ADVANCED_FACE('',(#2241),#1512,.T.);
#13720=ADVANCED_FACE('',(#2242),#1513,.T.);
#13721=ADVANCED_FACE('',(#2243),#1514,.T.);
#13722=ADVANCED_FACE('',(#2244),#1515,.F.);
#13723=ADVANCED_FACE('',(#2245),#1516,.T.);
#13724=ADVANCED_FACE('',(#2246),#1517,.T.);
#13725=ADVANCED_FACE('',(#2247),#1518,.T.);
#13726=ADVANCED_FACE('',(#2248),#1519,.F.);
#13727=ADVANCED_FACE('',(#2249),#13007,.F.);
#13728=ADVANCED_FACE('',(#2250),#13008,.T.);
#13729=ADVANCED_FACE('',(#2251,#1039),#1520,.T.);
#13730=ADVANCED_FACE('',(#2252,#1040),#1521,.F.);
#13731=ADVANCED_FACE('',(#2253),#1522,.T.);
#13732=ADVANCED_FACE('',(#2254),#634,.T.);
#13733=ADVANCED_FACE('',(#2255),#13009,.T.);
#13734=ADVANCED_FACE('',(#2256),#635,.T.);
#13735=ADVANCED_FACE('',(#2257,#1041),#1523,.T.);
#13736=ADVANCED_FACE('',(#2258),#636,.T.);
#13737=ADVANCED_FACE('',(#2259),#13010,.T.);
#13738=ADVANCED_FACE('',(#2260),#637,.T.);
#13739=ADVANCED_FACE('',(#2261),#1524,.T.);
#13740=ADVANCED_FACE('',(#2262),#1525,.F.);
#13741=ADVANCED_FACE('',(#2263),#1526,.F.);
#13742=ADVANCED_FACE('',(#2264),#1527,.F.);
#13743=ADVANCED_FACE('',(#2265),#1528,.F.);
#13744=ADVANCED_FACE('',(#2266),#1529,.F.);
#13745=ADVANCED_FACE('',(#2267),#1530,.F.);
#13746=ADVANCED_FACE('',(#2268),#1531,.F.);
#13747=ADVANCED_FACE('',(#2269),#1532,.F.);
#13748=ADVANCED_FACE('',(#2270),#13011,.F.);
#13749=ADVANCED_FACE('',(#2271),#13012,.T.);
#13750=ADVANCED_FACE('',(#2272,#1042),#1533,.T.);
#13751=ADVANCED_FACE('',(#2273,#1043),#1534,.F.);
#13752=CLOSED_SHELL('',(#13013,#13014,#13015,#13016,#13017,#13018,#13019,
#13020,#13021,#13022));
#13753=CLOSED_SHELL('',(#13023,#13024,#13025,#13026,#13027,#13028));
#13754=CLOSED_SHELL('',(#13029,#13030,#13031,#13032,#13033,#13034));
#13755=CLOSED_SHELL('',(#13035,#13036,#13037,#13038,#13039,#13040,#13041,
#13042,#13043,#13044,#13045,#13046,#13047,#13048,#13049,#13050,#13051,#13052,
#13053,#13054,#13055,#13056));
#13756=CLOSED_SHELL('',(#13057,#13058,#13059,#13060,#13061,#13062,#13063,
#13064,#13065,#13066,#13067,#13068));
#13757=CLOSED_SHELL('',(#13069,#13070,#13071,#13072,#13073,#13074));
#13758=CLOSED_SHELL('',(#13075,#13076,#13077,#13078,#13079,#13080,#13081,
#13082,#13083,#13084,#13085,#13086));
#13759=CLOSED_SHELL('',(#13087,#13088,#13089,#13090,#13091,#13092));
#13760=CLOSED_SHELL('',(#13093,#13094,#13095,#13096,#13097,#13098,#13099,
#13100,#13101,#13102,#13103,#13104,#13105,#13106,#13107,#13108,#13109));
#13761=CLOSED_SHELL('',(#13110,#13111,#13112,#13113,#13114,#13115,#13116,
#13117,#13118,#13119));
#13762=CLOSED_SHELL('',(#13120,#13121,#13122,#13123,#13124,#13125,#13126,
#13127,#13128,#13129));
#13763=CLOSED_SHELL('',(#13130,#13131,#13132,#13133,#13134,#13135,#13136,
#13137,#13138,#13139,#13140,#13141,#13142,#13143,#13144,#13145,#13146));
#13764=CLOSED_SHELL('',(#13147,#13148,#13149,#13150,#13151,#13152,#13153,
#13154,#13155,#13156));
#13765=CLOSED_SHELL('',(#13157,#13158,#13159,#13160,#13161,#13162,#13163,
#13164,#13165,#13166));
#13766=CLOSED_SHELL('',(#13167,#13168,#13169,#13170,#13171,#13172,#13173,
#13174,#13175,#13176,#13177,#13178,#13179,#13180,#13181,#13182,#13183,#13184,
#13185,#13186,#13187,#13188,#13189,#13190,#13191,#13192,#13193,#13194,#13195,
#13196,#13197,#13198,#13199,#13200,#13201,#13202,#13203,#13204,#13205,#13206,
#13207,#13208,#13209,#13210,#13211,#13212,#13213));
#13767=CLOSED_SHELL('',(#13214,#13215,#13216,#13217,#13218,#13219,#13220,
#13221,#13222,#13223,#13224,#13225,#13226,#13227));
#13768=CLOSED_SHELL('',(#13228,#13229,#13230,#13231,#13232));
#13769=CLOSED_SHELL('',(#13233,#13234,#13235,#13236,#13237,#13238,#13239,
#13240,#13241,#13242,#13243,#13244,#13245,#13246,#13247,#13248,#13249,#13250,
#13251,#13252,#13253,#13254,#13255,#13256,#13257,#13258));
#13770=CLOSED_SHELL('',(#13259,#13260,#13261,#13262,#13263,#13264,#13265,
#13266,#13267));
#13771=CLOSED_SHELL('',(#13268,#13269,#13270,#13271,#13272,#13273,#13274,
#13275));
#13772=CLOSED_SHELL('',(#13276,#13277,#13278,#13279,#13280,#13281,#13282,
#13283));
#13773=CLOSED_SHELL('',(#13284,#13285,#13286,#13287,#13288,#13289,#13290,
#13291));
#13774=CLOSED_SHELL('',(#13292));
#13775=CLOSED_SHELL('',(#13293));
#13776=CLOSED_SHELL('',(#13294));
#13777=CLOSED_SHELL('',(#13295));
#13778=CLOSED_SHELL('',(#13296));
#13779=CLOSED_SHELL('',(#13297));
#13780=CLOSED_SHELL('',(#13298));
#13781=CLOSED_SHELL('',(#13299,#13300,#13301,#13302,#13303,#13304,#13305,
#13306,#13307,#13308,#13309,#13310,#13311,#13312,#13313,#13314,#13315));
#13782=CLOSED_SHELL('',(#13316,#13317,#13318,#13319));
#13783=CLOSED_SHELL('',(#13320,#13321,#13322,#13323));
#13784=CLOSED_SHELL('',(#13324,#13325,#13326,#13327,#13328,#13329,#13330,
#13331));
#13785=CLOSED_SHELL('',(#13332,#13333,#13334,#13335,#13336,#13337,#13338,
#13339));
#13786=CLOSED_SHELL('',(#13340,#13341,#13342,#13343,#13344,#13345,#13346,
#13347,#13348,#13349,#13350,#13351,#13352,#13353));
#13787=CLOSED_SHELL('',(#13354,#13355,#13356,#13357,#13358,#13359,#13360,
#13361,#13362,#13363,#13364,#13365,#13366,#13367,#13368,#13369,#13370,#13371,
#13372,#13373,#13374,#13375,#13376,#13377,#13378,#13379,#13380,#13381,#13382,
#13383,#13384,#13385,#13386,#13387,#13388,#13389,#13390,#13391,#13392,#13393,
#13394,#13395,#13396,#13397,#13398,#13399,#13400,#13401,#13402,#13403,#13404,
#13405,#13406,#13407,#13408,#13409,#13410,#13411,#13412,#13413,#13414,#13415,
#13416,#13417,#13418,#13419,#13420,#13421,#13422,#13423,#13424,#13425,#13426,
#13427,#13428,#13429,#13430,#13431,#13432,#13433,#13434,#13435,#13436,#13437,
#13438,#13439,#13440,#13441,#13442,#13443,#13444,#13445,#13446,#13447,#13448,
#13449,#13450,#13451,#13452,#13453,#13454,#13455,#13456,#13457,#13458,#13459,
#13460,#13461,#13462,#13463,#13464,#13465,#13466,#13467,#13468,#13469,#13470,
#13471,#13472,#13473,#13474,#13475,#13476,#13477,#13478,#13479,#13480,#13481,
#13482,#13483,#13484,#13485,#13486,#13487,#13488,#13489,#13490,#13491));
#13788=CLOSED_SHELL('',(#13492,#13493,#13494,#13495,#13496,#13497,#13498,
#13499,#13500,#13501,#13502,#13503,#13504,#13505,#13506,#13507,#13508,#13509,
#13510,#13511,#13512,#13513));
#13789=CLOSED_SHELL('',(#13514,#13515,#13516,#13517,#13518,#13519,#13520,
#13521,#13522,#13523));
#13790=CLOSED_SHELL('',(#13524,#13525,#13526,#13527,#13528,#13529,#13530,
#13531,#13532,#13533));
#13791=CLOSED_SHELL('',(#13534,#13535,#13536,#13537,#13538,#13539,#13540,
#13541));
#13792=CLOSED_SHELL('',(#13542,#13543,#13544,#13545,#13546,#13547,#13548,
#13549));
#13793=CLOSED_SHELL('',(#13550,#13551,#13552,#13553,#13554,#13555,#13556,
#13557,#13558,#13559,#13560,#13561,#13562,#13563,#13564,#13565,#13566,#13567,
#13568,#13569,#13570));
#13794=CLOSED_SHELL('',(#13571,#13572,#13573,#13574));
#13795=CLOSED_SHELL('',(#13575,#13576,#13577,#13578));
#13796=CLOSED_SHELL('',(#13579,#13580,#13581,#13582));
#13797=CLOSED_SHELL('',(#13583,#13584,#13585,#13586));
#13798=CLOSED_SHELL('',(#13587,#13588,#13589,#13590));
#13799=CLOSED_SHELL('',(#13591,#13592,#13593,#13594));
#13800=CLOSED_SHELL('',(#13595,#13596,#13597,#13598,#13599,#13600,#13601,
#13602,#13603,#13604,#13605,#13606,#13607));
#13801=CLOSED_SHELL('',(#13608,#13609,#13610,#13611));
#13802=CLOSED_SHELL('',(#13612,#13613,#13614,#13615,#13616,#13617,#13618,
#13619,#13620,#13621,#13622,#13623,#13624,#13625,#13626,#13627,#13628,#13629,
#13630,#13631,#13632,#13633,#13634,#13635,#13636,#13637,#13638,#13639,#13640,
#13641,#13642,#13643,#13644,#13645,#13646,#13647,#13648,#13649,#13650,#13651,
#13652,#13653,#13654,#13655,#13656,#13657,#13658,#13659,#13660,#13661,#13662,
#13663,#13664,#13665,#13666,#13667,#13668,#13669,#13670,#13671,#13672,#13673,
#13674,#13675,#13676,#13677,#13678,#13679,#13680,#13681,#13682,#13683,#13684,
#13685,#13686,#13687,#13688,#13689,#13690,#13691,#13692,#13693,#13694,#13695,
#13696,#13697,#13698,#13699));
#13803=CLOSED_SHELL('',(#13700,#13701,#13702,#13703,#13704,#13705,#13706,
#13707,#13708));
#13804=CLOSED_SHELL('',(#13709,#13710,#13711,#13712,#13713,#13714,#13715,
#13716));
#13805=CLOSED_SHELL('',(#13717,#13718,#13719,#13720,#13721,#13722,#13723,
#13724,#13725,#13726));
#13806=CLOSED_SHELL('',(#13727,#13728,#13729,#13730));
#13807=CLOSED_SHELL('',(#13731,#13732,#13733,#13734,#13735,#13736,#13737,
#13738,#13739));
#13808=CLOSED_SHELL('',(#13740,#13741,#13742,#13743,#13744,#13745,#13746,
#13747));
#13809=CLOSED_SHELL('',(#13748,#13749,#13750,#13751));
#13810=DERIVED_UNIT_ELEMENT(#13902,1.);
#13811=DERIVED_UNIT_ELEMENT(#34853,-3.);
#13812=DERIVED_UNIT_ELEMENT(#13902,1.);
#13813=DERIVED_UNIT_ELEMENT(#34853,-3.);
#13814=DERIVED_UNIT_ELEMENT(#13902,1.);
#13815=DERIVED_UNIT_ELEMENT(#34853,-3.);
#13816=DERIVED_UNIT_ELEMENT(#13902,1.);
#13817=DERIVED_UNIT_ELEMENT(#34853,-3.);
#13818=DERIVED_UNIT_ELEMENT(#13902,1.);
#13819=DERIVED_UNIT_ELEMENT(#34853,-3.);
#13820=DERIVED_UNIT_ELEMENT(#13902,1.);
#13821=DERIVED_UNIT_ELEMENT(#34853,-3.);
#13822=DERIVED_UNIT_ELEMENT(#13902,1.);
#13823=DERIVED_UNIT_ELEMENT(#34853,-3.);
#13824=DERIVED_UNIT_ELEMENT(#13902,1.);
#13825=DERIVED_UNIT_ELEMENT(#34853,-3.);
#13826=DERIVED_UNIT_ELEMENT(#13902,1.);
#13827=DERIVED_UNIT_ELEMENT(#34853,-3.);
#13828=DERIVED_UNIT_ELEMENT(#13902,1.);
#13829=DERIVED_UNIT_ELEMENT(#34853,-3.);
#13830=DERIVED_UNIT_ELEMENT(#13902,1.);
#13831=DERIVED_UNIT_ELEMENT(#34853,-3.);
#13832=DERIVED_UNIT_ELEMENT(#13902,1.);
#13833=DERIVED_UNIT_ELEMENT(#34853,-3.);
#13834=DERIVED_UNIT_ELEMENT(#13902,1.);
#13835=DERIVED_UNIT_ELEMENT(#34853,-3.);
#13836=DERIVED_UNIT_ELEMENT(#13902,1.);
#13837=DERIVED_UNIT_ELEMENT(#34853,-3.);
#13838=DERIVED_UNIT_ELEMENT(#13902,1.);
#13839=DERIVED_UNIT_ELEMENT(#34853,-3.);
#13840=DERIVED_UNIT_ELEMENT(#13902,1.);
#13841=DERIVED_UNIT_ELEMENT(#34853,-3.);
#13842=DERIVED_UNIT_ELEMENT(#13902,1.);
#13843=DERIVED_UNIT_ELEMENT(#34853,-3.);
#13844=DERIVED_UNIT_ELEMENT(#13902,1.);
#13845=DERIVED_UNIT_ELEMENT(#34853,-3.);
#13846=DERIVED_UNIT_ELEMENT(#13902,1.);
#13847=DERIVED_UNIT_ELEMENT(#34853,-3.);
#13848=DERIVED_UNIT_ELEMENT(#13902,1.);
#13849=DERIVED_UNIT_ELEMENT(#34853,-3.);
#13850=DERIVED_UNIT_ELEMENT(#13902,1.);
#13851=DERIVED_UNIT_ELEMENT(#34853,-3.);
#13852=DERIVED_UNIT_ELEMENT(#13902,1.);
#13853=DERIVED_UNIT_ELEMENT(#34853,-3.);
#13854=DERIVED_UNIT_ELEMENT(#13902,1.);
#13855=DERIVED_UNIT_ELEMENT(#34853,-3.);
#13856=DERIVED_UNIT_ELEMENT(#13902,1.);
#13857=DERIVED_UNIT_ELEMENT(#34853,-3.);
#13858=DERIVED_UNIT_ELEMENT(#13902,1.);
#13859=DERIVED_UNIT_ELEMENT(#34853,-3.);
#13860=DERIVED_UNIT_ELEMENT(#13902,1.);
#13861=DERIVED_UNIT_ELEMENT(#34853,-3.);
#13862=DERIVED_UNIT_ELEMENT(#13902,1.);
#13863=DERIVED_UNIT_ELEMENT(#34853,-3.);
#13864=DERIVED_UNIT_ELEMENT(#13902,1.);
#13865=DERIVED_UNIT_ELEMENT(#34853,-3.);
#13866=DERIVED_UNIT_ELEMENT(#13902,1.);
#13867=DERIVED_UNIT_ELEMENT(#34853,-3.);
#13868=DERIVED_UNIT_ELEMENT(#13902,1.);
#13869=DERIVED_UNIT_ELEMENT(#34853,-3.);
#13870=DERIVED_UNIT_ELEMENT(#13902,1.);
#13871=DERIVED_UNIT_ELEMENT(#34853,-3.);
#13872=DERIVED_UNIT_ELEMENT(#13902,1.);
#13873=DERIVED_UNIT_ELEMENT(#34853,-3.);
#13874=DERIVED_UNIT_ELEMENT(#13902,1.);
#13875=DERIVED_UNIT_ELEMENT(#34853,-3.);
#13876=DERIVED_UNIT_ELEMENT(#13902,1.);
#13877=DERIVED_UNIT_ELEMENT(#34853,-3.);
#13878=DERIVED_UNIT_ELEMENT(#13902,1.);
#13879=DERIVED_UNIT_ELEMENT(#34853,-3.);
#13880=DERIVED_UNIT_ELEMENT(#13902,1.);
#13881=DERIVED_UNIT_ELEMENT(#34853,-3.);
#13882=DERIVED_UNIT_ELEMENT(#13902,1.);
#13883=DERIVED_UNIT_ELEMENT(#34853,-3.);
#13884=DERIVED_UNIT_ELEMENT(#13902,1.);
#13885=DERIVED_UNIT_ELEMENT(#34853,-3.);
#13886=DERIVED_UNIT_ELEMENT(#13902,1.);
#13887=DERIVED_UNIT_ELEMENT(#34853,-3.);
#13888=DERIVED_UNIT_ELEMENT(#13902,1.);
#13889=DERIVED_UNIT_ELEMENT(#34853,-3.);
#13890=DERIVED_UNIT_ELEMENT(#13902,1.);
#13891=DERIVED_UNIT_ELEMENT(#34853,-3.);
#13892=DERIVED_UNIT_ELEMENT(#13902,1.);
#13893=DERIVED_UNIT_ELEMENT(#34853,-3.);
#13894=DERIVED_UNIT_ELEMENT(#13902,1.);
#13895=DERIVED_UNIT_ELEMENT(#34853,-3.);
#13896=DERIVED_UNIT_ELEMENT(#13902,1.);
#13897=DERIVED_UNIT_ELEMENT(#34853,-3.);
#13898=DERIVED_UNIT_ELEMENT(#13902,1.);
#13899=DERIVED_UNIT_ELEMENT(#34853,-3.);
#13900=DERIVED_UNIT_ELEMENT(#13902,1.);
#13901=DERIVED_UNIT_ELEMENT(#34853,-3.);
#13902=(
MASS_UNIT()
NAMED_UNIT(*)
SI_UNIT(.KILO.,.GRAM.)
);
#13903=DERIVED_UNIT((#13810,#13811));
#13904=DERIVED_UNIT((#13812,#13813));
#13905=DERIVED_UNIT((#13814,#13815));
#13906=DERIVED_UNIT((#13816,#13817));
#13907=DERIVED_UNIT((#13818,#13819));
#13908=DERIVED_UNIT((#13820,#13821));
#13909=DERIVED_UNIT((#13822,#13823));
#13910=DERIVED_UNIT((#13824,#13825));
#13911=DERIVED_UNIT((#13826,#13827));
#13912=DERIVED_UNIT((#13828,#13829));
#13913=DERIVED_UNIT((#13830,#13831));
#13914=DERIVED_UNIT((#13832,#13833));
#13915=DERIVED_UNIT((#13834,#13835));
#13916=DERIVED_UNIT((#13836,#13837));
#13917=DERIVED_UNIT((#13838,#13839));
#13918=DERIVED_UNIT((#13840,#13841));
#13919=DERIVED_UNIT((#13842,#13843));
#13920=DERIVED_UNIT((#13844,#13845));
#13921=DERIVED_UNIT((#13846,#13847));
#13922=DERIVED_UNIT((#13848,#13849));
#13923=DERIVED_UNIT((#13850,#13851));
#13924=DERIVED_UNIT((#13852,#13853));
#13925=DERIVED_UNIT((#13854,#13855));
#13926=DERIVED_UNIT((#13856,#13857));
#13927=DERIVED_UNIT((#13858,#13859));
#13928=DERIVED_UNIT((#13860,#13861));
#13929=DERIVED_UNIT((#13862,#13863));
#13930=DERIVED_UNIT((#13864,#13865));
#13931=DERIVED_UNIT((#13866,#13867));
#13932=DERIVED_UNIT((#13868,#13869));
#13933=DERIVED_UNIT((#13870,#13871));
#13934=DERIVED_UNIT((#13872,#13873));
#13935=DERIVED_UNIT((#13874,#13875));
#13936=DERIVED_UNIT((#13876,#13877));
#13937=DERIVED_UNIT((#13878,#13879));
#13938=DERIVED_UNIT((#13880,#13881));
#13939=DERIVED_UNIT((#13882,#13883));
#13940=DERIVED_UNIT((#13884,#13885));
#13941=DERIVED_UNIT((#13886,#13887));
#13942=DERIVED_UNIT((#13888,#13889));
#13943=DERIVED_UNIT((#13890,#13891));
#13944=DERIVED_UNIT((#13892,#13893));
#13945=DERIVED_UNIT((#13894,#13895));
#13946=DERIVED_UNIT((#13896,#13897));
#13947=DERIVED_UNIT((#13898,#13899));
#13948=DERIVED_UNIT((#13900,#13901));
#13949=MEASURE_REPRESENTATION_ITEM('density measure',
POSITIVE_RATIO_MEASURE(7850.),#13903);
#13950=MEASURE_REPRESENTATION_ITEM('density measure',
POSITIVE_RATIO_MEASURE(7850.),#13904);
#13951=MEASURE_REPRESENTATION_ITEM('density measure',
POSITIVE_RATIO_MEASURE(7850.),#13905);
#13952=MEASURE_REPRESENTATION_ITEM('density measure',
POSITIVE_RATIO_MEASURE(7850.),#13906);
#13953=MEASURE_REPRESENTATION_ITEM('density measure',
POSITIVE_RATIO_MEASURE(7850.),#13907);
#13954=MEASURE_REPRESENTATION_ITEM('density measure',
POSITIVE_RATIO_MEASURE(7850.),#13908);
#13955=MEASURE_REPRESENTATION_ITEM('density measure',
POSITIVE_RATIO_MEASURE(7850.),#13909);
#13956=MEASURE_REPRESENTATION_ITEM('density measure',
POSITIVE_RATIO_MEASURE(7850.),#13910);
#13957=MEASURE_REPRESENTATION_ITEM('density measure',
POSITIVE_RATIO_MEASURE(7850.),#13911);
#13958=MEASURE_REPRESENTATION_ITEM('density measure',
POSITIVE_RATIO_MEASURE(7850.),#13912);
#13959=MEASURE_REPRESENTATION_ITEM('density measure',
POSITIVE_RATIO_MEASURE(7850.),#13913);
#13960=MEASURE_REPRESENTATION_ITEM('density measure',
POSITIVE_RATIO_MEASURE(7850.),#13914);
#13961=MEASURE_REPRESENTATION_ITEM('density measure',
POSITIVE_RATIO_MEASURE(7850.),#13915);
#13962=MEASURE_REPRESENTATION_ITEM('density measure',
POSITIVE_RATIO_MEASURE(7850.),#13916);
#13963=MEASURE_REPRESENTATION_ITEM('density measure',
POSITIVE_RATIO_MEASURE(7850.),#13917);
#13964=MEASURE_REPRESENTATION_ITEM('density measure',
POSITIVE_RATIO_MEASURE(7850.),#13918);
#13965=MEASURE_REPRESENTATION_ITEM('density measure',
POSITIVE_RATIO_MEASURE(7850.),#13919);
#13966=MEASURE_REPRESENTATION_ITEM('density measure',
POSITIVE_RATIO_MEASURE(7850.),#13920);
#13967=MEASURE_REPRESENTATION_ITEM('density measure',
POSITIVE_RATIO_MEASURE(7850.),#13921);
#13968=MEASURE_REPRESENTATION_ITEM('density measure',
POSITIVE_RATIO_MEASURE(7850.),#13922);
#13969=MEASURE_REPRESENTATION_ITEM('density measure',
POSITIVE_RATIO_MEASURE(7850.),#13923);
#13970=MEASURE_REPRESENTATION_ITEM('density measure',
POSITIVE_RATIO_MEASURE(7850.),#13924);
#13971=MEASURE_REPRESENTATION_ITEM('density measure',
POSITIVE_RATIO_MEASURE(7850.),#13925);
#13972=MEASURE_REPRESENTATION_ITEM('density measure',
POSITIVE_RATIO_MEASURE(7850.),#13926);
#13973=MEASURE_REPRESENTATION_ITEM('density measure',
POSITIVE_RATIO_MEASURE(7850.),#13927);
#13974=MEASURE_REPRESENTATION_ITEM('density measure',
POSITIVE_RATIO_MEASURE(7850.),#13928);
#13975=MEASURE_REPRESENTATION_ITEM('density measure',
POSITIVE_RATIO_MEASURE(7850.),#13929);
#13976=MEASURE_REPRESENTATION_ITEM('density measure',
POSITIVE_RATIO_MEASURE(7850.),#13930);
#13977=MEASURE_REPRESENTATION_ITEM('density measure',
POSITIVE_RATIO_MEASURE(7850.),#13931);
#13978=MEASURE_REPRESENTATION_ITEM('density measure',
POSITIVE_RATIO_MEASURE(7850.),#13932);
#13979=MEASURE_REPRESENTATION_ITEM('density measure',
POSITIVE_RATIO_MEASURE(7850.),#13933);
#13980=MEASURE_REPRESENTATION_ITEM('density measure',
POSITIVE_RATIO_MEASURE(7850.),#13934);
#13981=MEASURE_REPRESENTATION_ITEM('density measure',
POSITIVE_RATIO_MEASURE(7850.),#13935);
#13982=MEASURE_REPRESENTATION_ITEM('density measure',
POSITIVE_RATIO_MEASURE(7850.),#13936);
#13983=MEASURE_REPRESENTATION_ITEM('density measure',
POSITIVE_RATIO_MEASURE(7850.),#13937);
#13984=MEASURE_REPRESENTATION_ITEM('density measure',
POSITIVE_RATIO_MEASURE(7850.),#13938);
#13985=MEASURE_REPRESENTATION_ITEM('density measure',
POSITIVE_RATIO_MEASURE(7850.),#13939);
#13986=MEASURE_REPRESENTATION_ITEM('density measure',
POSITIVE_RATIO_MEASURE(7850.),#13940);
#13987=MEASURE_REPRESENTATION_ITEM('density measure',
POSITIVE_RATIO_MEASURE(7850.),#13941);
#13988=MEASURE_REPRESENTATION_ITEM('density measure',
POSITIVE_RATIO_MEASURE(7850.),#13942);
#13989=MEASURE_REPRESENTATION_ITEM('density measure',
POSITIVE_RATIO_MEASURE(7850.),#13943);
#13990=MEASURE_REPRESENTATION_ITEM('density measure',
POSITIVE_RATIO_MEASURE(7850.),#13944);
#13991=MEASURE_REPRESENTATION_ITEM('density measure',
POSITIVE_RATIO_MEASURE(7850.),#13945);
#13992=MEASURE_REPRESENTATION_ITEM('density measure',
POSITIVE_RATIO_MEASURE(7850.),#13946);
#13993=MEASURE_REPRESENTATION_ITEM('density measure',
POSITIVE_RATIO_MEASURE(7850.),#13947);
#13994=MEASURE_REPRESENTATION_ITEM('density measure',
POSITIVE_RATIO_MEASURE(7850.),#13948);
#13995=PROPERTY_DEFINITION_REPRESENTATION(#14225,#14087);
#13996=PROPERTY_DEFINITION_REPRESENTATION(#14226,#14088);
#13997=PROPERTY_DEFINITION_REPRESENTATION(#14227,#14089);
#13998=PROPERTY_DEFINITION_REPRESENTATION(#14228,#14090);
#13999=PROPERTY_DEFINITION_REPRESENTATION(#14229,#14091);
#14000=PROPERTY_DEFINITION_REPRESENTATION(#14230,#14092);
#14001=PROPERTY_DEFINITION_REPRESENTATION(#14231,#14093);
#14002=PROPERTY_DEFINITION_REPRESENTATION(#14232,#14094);
#14003=PROPERTY_DEFINITION_REPRESENTATION(#14233,#14095);
#14004=PROPERTY_DEFINITION_REPRESENTATION(#14234,#14096);
#14005=PROPERTY_DEFINITION_REPRESENTATION(#14235,#14097);
#14006=PROPERTY_DEFINITION_REPRESENTATION(#14236,#14098);
#14007=PROPERTY_DEFINITION_REPRESENTATION(#14237,#14099);
#14008=PROPERTY_DEFINITION_REPRESENTATION(#14238,#14100);
#14009=PROPERTY_DEFINITION_REPRESENTATION(#14239,#14101);
#14010=PROPERTY_DEFINITION_REPRESENTATION(#14240,#14102);
#14011=PROPERTY_DEFINITION_REPRESENTATION(#14241,#14103);
#14012=PROPERTY_DEFINITION_REPRESENTATION(#14242,#14104);
#14013=PROPERTY_DEFINITION_REPRESENTATION(#14243,#14105);
#14014=PROPERTY_DEFINITION_REPRESENTATION(#14244,#14106);
#14015=PROPERTY_DEFINITION_REPRESENTATION(#14245,#14107);
#14016=PROPERTY_DEFINITION_REPRESENTATION(#14246,#14108);
#14017=PROPERTY_DEFINITION_REPRESENTATION(#14247,#14109);
#14018=PROPERTY_DEFINITION_REPRESENTATION(#14248,#14110);
#14019=PROPERTY_DEFINITION_REPRESENTATION(#14249,#14111);
#14020=PROPERTY_DEFINITION_REPRESENTATION(#14250,#14112);
#14021=PROPERTY_DEFINITION_REPRESENTATION(#14251,#14113);
#14022=PROPERTY_DEFINITION_REPRESENTATION(#14252,#14114);
#14023=PROPERTY_DEFINITION_REPRESENTATION(#14253,#14115);
#14024=PROPERTY_DEFINITION_REPRESENTATION(#14254,#14116);
#14025=PROPERTY_DEFINITION_REPRESENTATION(#14255,#14117);
#14026=PROPERTY_DEFINITION_REPRESENTATION(#14256,#14118);
#14027=PROPERTY_DEFINITION_REPRESENTATION(#14257,#14119);
#14028=PROPERTY_DEFINITION_REPRESENTATION(#14258,#14120);
#14029=PROPERTY_DEFINITION_REPRESENTATION(#14259,#14121);
#14030=PROPERTY_DEFINITION_REPRESENTATION(#14260,#14122);
#14031=PROPERTY_DEFINITION_REPRESENTATION(#14261,#14123);
#14032=PROPERTY_DEFINITION_REPRESENTATION(#14262,#14124);
#14033=PROPERTY_DEFINITION_REPRESENTATION(#14263,#14125);
#14034=PROPERTY_DEFINITION_REPRESENTATION(#14264,#14126);
#14035=PROPERTY_DEFINITION_REPRESENTATION(#14265,#14127);
#14036=PROPERTY_DEFINITION_REPRESENTATION(#14266,#14128);
#14037=PROPERTY_DEFINITION_REPRESENTATION(#14267,#14129);
#14038=PROPERTY_DEFINITION_REPRESENTATION(#14268,#14130);
#14039=PROPERTY_DEFINITION_REPRESENTATION(#14269,#14131);
#14040=PROPERTY_DEFINITION_REPRESENTATION(#14270,#14132);
#14041=PROPERTY_DEFINITION_REPRESENTATION(#14271,#14133);
#14042=PROPERTY_DEFINITION_REPRESENTATION(#14272,#14134);
#14043=PROPERTY_DEFINITION_REPRESENTATION(#14273,#14135);
#14044=PROPERTY_DEFINITION_REPRESENTATION(#14274,#14136);
#14045=PROPERTY_DEFINITION_REPRESENTATION(#14275,#14137);
#14046=PROPERTY_DEFINITION_REPRESENTATION(#14276,#14138);
#14047=PROPERTY_DEFINITION_REPRESENTATION(#14277,#14139);
#14048=PROPERTY_DEFINITION_REPRESENTATION(#14278,#14140);
#14049=PROPERTY_DEFINITION_REPRESENTATION(#14279,#14141);
#14050=PROPERTY_DEFINITION_REPRESENTATION(#14280,#14142);
#14051=PROPERTY_DEFINITION_REPRESENTATION(#14281,#14143);
#14052=PROPERTY_DEFINITION_REPRESENTATION(#14282,#14144);
#14053=PROPERTY_DEFINITION_REPRESENTATION(#14283,#14145);
#14054=PROPERTY_DEFINITION_REPRESENTATION(#14284,#14146);
#14055=PROPERTY_DEFINITION_REPRESENTATION(#14285,#14147);
#14056=PROPERTY_DEFINITION_REPRESENTATION(#14286,#14148);
#14057=PROPERTY_DEFINITION_REPRESENTATION(#14287,#14149);
#14058=PROPERTY_DEFINITION_REPRESENTATION(#14288,#14150);
#14059=PROPERTY_DEFINITION_REPRESENTATION(#14289,#14151);
#14060=PROPERTY_DEFINITION_REPRESENTATION(#14290,#14152);
#14061=PROPERTY_DEFINITION_REPRESENTATION(#14291,#14153);
#14062=PROPERTY_DEFINITION_REPRESENTATION(#14292,#14154);
#14063=PROPERTY_DEFINITION_REPRESENTATION(#14293,#14155);
#14064=PROPERTY_DEFINITION_REPRESENTATION(#14294,#14156);
#14065=PROPERTY_DEFINITION_REPRESENTATION(#14295,#14157);
#14066=PROPERTY_DEFINITION_REPRESENTATION(#14296,#14158);
#14067=PROPERTY_DEFINITION_REPRESENTATION(#14297,#14159);
#14068=PROPERTY_DEFINITION_REPRESENTATION(#14298,#14160);
#14069=PROPERTY_DEFINITION_REPRESENTATION(#14299,#14161);
#14070=PROPERTY_DEFINITION_REPRESENTATION(#14300,#14162);
#14071=PROPERTY_DEFINITION_REPRESENTATION(#14301,#14163);
#14072=PROPERTY_DEFINITION_REPRESENTATION(#14302,#14164);
#14073=PROPERTY_DEFINITION_REPRESENTATION(#14303,#14165);
#14074=PROPERTY_DEFINITION_REPRESENTATION(#14304,#14166);
#14075=PROPERTY_DEFINITION_REPRESENTATION(#14305,#14167);
#14076=PROPERTY_DEFINITION_REPRESENTATION(#14306,#14168);
#14077=PROPERTY_DEFINITION_REPRESENTATION(#14307,#14169);
#14078=PROPERTY_DEFINITION_REPRESENTATION(#14308,#14170);
#14079=PROPERTY_DEFINITION_REPRESENTATION(#14309,#14171);
#14080=PROPERTY_DEFINITION_REPRESENTATION(#14310,#14172);
#14081=PROPERTY_DEFINITION_REPRESENTATION(#14311,#14173);
#14082=PROPERTY_DEFINITION_REPRESENTATION(#14312,#14174);
#14083=PROPERTY_DEFINITION_REPRESENTATION(#14313,#14175);
#14084=PROPERTY_DEFINITION_REPRESENTATION(#14314,#14176);
#14085=PROPERTY_DEFINITION_REPRESENTATION(#14315,#14177);
#14086=PROPERTY_DEFINITION_REPRESENTATION(#14316,#14178);
#14087=REPRESENTATION('material name',(#14179),#34800);
#14088=REPRESENTATION('density',(#13949),#34800);
#14089=REPRESENTATION('material name',(#14180),#34801);
#14090=REPRESENTATION('density',(#13950),#34801);
#14091=REPRESENTATION('material name',(#14181),#34802);
#14092=REPRESENTATION('density',(#13951),#34802);
#14093=REPRESENTATION('material name',(#14182),#34803);
#14094=REPRESENTATION('density',(#13952),#34803);
#14095=REPRESENTATION('material name',(#14183),#34804);
#14096=REPRESENTATION('density',(#13953),#34804);
#14097=REPRESENTATION('material name',(#14184),#34805);
#14098=REPRESENTATION('density',(#13954),#34805);
#14099=REPRESENTATION('material name',(#14185),#34806);
#14100=REPRESENTATION('density',(#13955),#34806);
#14101=REPRESENTATION('material name',(#14186),#34807);
#14102=REPRESENTATION('density',(#13956),#34807);
#14103=REPRESENTATION('material name',(#14187),#34808);
#14104=REPRESENTATION('density',(#13957),#34808);
#14105=REPRESENTATION('material name',(#14188),#34809);
#14106=REPRESENTATION('density',(#13958),#34809);
#14107=REPRESENTATION('material name',(#14189),#34810);
#14108=REPRESENTATION('density',(#13959),#34810);
#14109=REPRESENTATION('material name',(#14190),#34811);
#14110=REPRESENTATION('density',(#13960),#34811);
#14111=REPRESENTATION('material name',(#14191),#34812);
#14112=REPRESENTATION('density',(#13961),#34812);
#14113=REPRESENTATION('material name',(#14192),#34813);
#14114=REPRESENTATION('density',(#13962),#34813);
#14115=REPRESENTATION('material name',(#14193),#34814);
#14116=REPRESENTATION('density',(#13963),#34814);
#14117=REPRESENTATION('material name',(#14194),#34815);
#14118=REPRESENTATION('density',(#13964),#34815);
#14119=REPRESENTATION('material name',(#14195),#34816);
#14120=REPRESENTATION('density',(#13965),#34816);
#14121=REPRESENTATION('material name',(#14196),#34817);
#14122=REPRESENTATION('density',(#13966),#34817);
#14123=REPRESENTATION('material name',(#14197),#34818);
#14124=REPRESENTATION('density',(#13967),#34818);
#14125=REPRESENTATION('material name',(#14198),#34820);
#14126=REPRESENTATION('density',(#13968),#34820);
#14127=REPRESENTATION('material name',(#14199),#34821);
#14128=REPRESENTATION('density',(#13969),#34821);
#14129=REPRESENTATION('material name',(#14200),#34822);
#14130=REPRESENTATION('density',(#13970),#34822);
#14131=REPRESENTATION('material name',(#14201),#34823);
#14132=REPRESENTATION('density',(#13971),#34823);
#14133=REPRESENTATION('material name',(#14202),#34824);
#14134=REPRESENTATION('density',(#13972),#34824);
#14135=REPRESENTATION('material name',(#14203),#34825);
#14136=REPRESENTATION('density',(#13973),#34825);
#14137=REPRESENTATION('material name',(#14204),#34827);
#14138=REPRESENTATION('density',(#13974),#34827);
#14139=REPRESENTATION('material name',(#14205),#34828);
#14140=REPRESENTATION('density',(#13975),#34828);
#14141=REPRESENTATION('material name',(#14206),#34830);
#14142=REPRESENTATION('density',(#13976),#34830);
#14143=REPRESENTATION('material name',(#14207),#34831);
#14144=REPRESENTATION('density',(#13977),#34831);
#14145=REPRESENTATION('material name',(#14208),#34832);
#14146=REPRESENTATION('density',(#13978),#34832);
#14147=REPRESENTATION('material name',(#14209),#34833);
#14148=REPRESENTATION('density',(#13979),#34833);
#14149=REPRESENTATION('material name',(#14210),#34835);
#14150=REPRESENTATION('density',(#13980),#34835);
#14151=REPRESENTATION('material name',(#14211),#34836);
#14152=REPRESENTATION('density',(#13981),#34836);
#14153=REPRESENTATION('material name',(#14212),#34837);
#14154=REPRESENTATION('density',(#13982),#34837);
#14155=REPRESENTATION('material name',(#14213),#34838);
#14156=REPRESENTATION('density',(#13983),#34838);
#14157=REPRESENTATION('material name',(#14214),#34839);
#14158=REPRESENTATION('density',(#13984),#34839);
#14159=REPRESENTATION('material name',(#14215),#34840);
#14160=REPRESENTATION('density',(#13985),#34840);
#14161=REPRESENTATION('material name',(#14216),#34841);
#14162=REPRESENTATION('density',(#13986),#34841);
#14163=REPRESENTATION('material name',(#14217),#34842);
#14164=REPRESENTATION('density',(#13987),#34842);
#14165=REPRESENTATION('material name',(#14218),#34843);
#14166=REPRESENTATION('density',(#13988),#34843);
#14167=REPRESENTATION('material name',(#14219),#34844);
#14168=REPRESENTATION('density',(#13989),#34844);
#14169=REPRESENTATION('material name',(#14220),#34845);
#14170=REPRESENTATION('density',(#13990),#34845);
#14171=REPRESENTATION('material name',(#14221),#34846);
#14172=REPRESENTATION('density',(#13991),#34846);
#14173=REPRESENTATION('material name',(#14222),#34847);
#14174=REPRESENTATION('density',(#13992),#34847);
#14175=REPRESENTATION('material name',(#14223),#34848);
#14176=REPRESENTATION('density',(#13993),#34848);
#14177=REPRESENTATION('material name',(#14224),#34850);
#14178=REPRESENTATION('density',(#13994),#34850);
#14179=DESCRIPTIVE_REPRESENTATION_ITEM('Steel','Steel');
#14180=DESCRIPTIVE_REPRESENTATION_ITEM('Steel','Steel');
#14181=DESCRIPTIVE_REPRESENTATION_ITEM('Steel','Steel');
#14182=DESCRIPTIVE_REPRESENTATION_ITEM('Steel','Steel');
#14183=DESCRIPTIVE_REPRESENTATION_ITEM('Steel','Steel');
#14184=DESCRIPTIVE_REPRESENTATION_ITEM('Steel','Steel');
#14185=DESCRIPTIVE_REPRESENTATION_ITEM('Steel','Steel');
#14186=DESCRIPTIVE_REPRESENTATION_ITEM('Steel','Steel');
#14187=DESCRIPTIVE_REPRESENTATION_ITEM('Steel','Steel');
#14188=DESCRIPTIVE_REPRESENTATION_ITEM('Steel','Steel');
#14189=DESCRIPTIVE_REPRESENTATION_ITEM('Steel','Steel');
#14190=DESCRIPTIVE_REPRESENTATION_ITEM('Steel','Steel');
#14191=DESCRIPTIVE_REPRESENTATION_ITEM('Steel','Steel');
#14192=DESCRIPTIVE_REPRESENTATION_ITEM('Steel','Steel');
#14193=DESCRIPTIVE_REPRESENTATION_ITEM('Steel','Steel');
#14194=DESCRIPTIVE_REPRESENTATION_ITEM('Steel','Steel');
#14195=DESCRIPTIVE_REPRESENTATION_ITEM('Steel','Steel');
#14196=DESCRIPTIVE_REPRESENTATION_ITEM('Steel','Steel');
#14197=DESCRIPTIVE_REPRESENTATION_ITEM('Steel','Steel');
#14198=DESCRIPTIVE_REPRESENTATION_ITEM('Steel','Steel');
#14199=DESCRIPTIVE_REPRESENTATION_ITEM('Steel','Steel');
#14200=DESCRIPTIVE_REPRESENTATION_ITEM('Steel','Steel');
#14201=DESCRIPTIVE_REPRESENTATION_ITEM('Steel','Steel');
#14202=DESCRIPTIVE_REPRESENTATION_ITEM('Steel','Steel');
#14203=DESCRIPTIVE_REPRESENTATION_ITEM('Steel','Steel');
#14204=DESCRIPTIVE_REPRESENTATION_ITEM('Steel','Steel');
#14205=DESCRIPTIVE_REPRESENTATION_ITEM('Steel','Steel');
#14206=DESCRIPTIVE_REPRESENTATION_ITEM('Steel','Steel');
#14207=DESCRIPTIVE_REPRESENTATION_ITEM('Steel','Steel');
#14208=DESCRIPTIVE_REPRESENTATION_ITEM('Steel','Steel');
#14209=DESCRIPTIVE_REPRESENTATION_ITEM('Steel','Steel');
#14210=DESCRIPTIVE_REPRESENTATION_ITEM('Steel','Steel');
#14211=DESCRIPTIVE_REPRESENTATION_ITEM('Steel','Steel');
#14212=DESCRIPTIVE_REPRESENTATION_ITEM('Steel','Steel');
#14213=DESCRIPTIVE_REPRESENTATION_ITEM('Steel','Steel');
#14214=DESCRIPTIVE_REPRESENTATION_ITEM('Steel','Steel');
#14215=DESCRIPTIVE_REPRESENTATION_ITEM('Steel','Steel');
#14216=DESCRIPTIVE_REPRESENTATION_ITEM('Steel','Steel');
#14217=DESCRIPTIVE_REPRESENTATION_ITEM('Steel','Steel');
#14218=DESCRIPTIVE_REPRESENTATION_ITEM('Steel','Steel');
#14219=DESCRIPTIVE_REPRESENTATION_ITEM('Steel','Steel');
#14220=DESCRIPTIVE_REPRESENTATION_ITEM('Steel','Steel');
#14221=DESCRIPTIVE_REPRESENTATION_ITEM('Steel','Steel');
#14222=DESCRIPTIVE_REPRESENTATION_ITEM('Steel','Steel');
#14223=DESCRIPTIVE_REPRESENTATION_ITEM('Steel','Steel');
#14224=DESCRIPTIVE_REPRESENTATION_ITEM('Steel','Steel');
#14225=PROPERTY_DEFINITION('material property','material name',#35129);
#14226=PROPERTY_DEFINITION('material property','density of part',#35129);
#14227=PROPERTY_DEFINITION('material property','material name',#35130);
#14228=PROPERTY_DEFINITION('material property','density of part',#35130);
#14229=PROPERTY_DEFINITION('material property','material name',#35131);
#14230=PROPERTY_DEFINITION('material property','density of part',#35131);
#14231=PROPERTY_DEFINITION('material property','material name',#35132);
#14232=PROPERTY_DEFINITION('material property','density of part',#35132);
#14233=PROPERTY_DEFINITION('material property','material name',#35133);
#14234=PROPERTY_DEFINITION('material property','density of part',#35133);
#14235=PROPERTY_DEFINITION('material property','material name',#35134);
#14236=PROPERTY_DEFINITION('material property','density of part',#35134);
#14237=PROPERTY_DEFINITION('material property','material name',#35135);
#14238=PROPERTY_DEFINITION('material property','density of part',#35135);
#14239=PROPERTY_DEFINITION('material property','material name',#35136);
#14240=PROPERTY_DEFINITION('material property','density of part',#35136);
#14241=PROPERTY_DEFINITION('material property','material name',#35137);
#14242=PROPERTY_DEFINITION('material property','density of part',#35137);
#14243=PROPERTY_DEFINITION('material property','material name',#35138);
#14244=PROPERTY_DEFINITION('material property','density of part',#35138);
#14245=PROPERTY_DEFINITION('material property','material name',#35139);
#14246=PROPERTY_DEFINITION('material property','density of part',#35139);
#14247=PROPERTY_DEFINITION('material property','material name',#35140);
#14248=PROPERTY_DEFINITION('material property','density of part',#35140);
#14249=PROPERTY_DEFINITION('material property','material name',#35141);
#14250=PROPERTY_DEFINITION('material property','density of part',#35141);
#14251=PROPERTY_DEFINITION('material property','material name',#35142);
#14252=PROPERTY_DEFINITION('material property','density of part',#35142);
#14253=PROPERTY_DEFINITION('material property','material name',#35143);
#14254=PROPERTY_DEFINITION('material property','density of part',#35143);
#14255=PROPERTY_DEFINITION('material property','material name',#35144);
#14256=PROPERTY_DEFINITION('material property','density of part',#35144);
#14257=PROPERTY_DEFINITION('material property','material name',#35145);
#14258=PROPERTY_DEFINITION('material property','density of part',#35145);
#14259=PROPERTY_DEFINITION('material property','material name',#35146);
#14260=PROPERTY_DEFINITION('material property','density of part',#35146);
#14261=PROPERTY_DEFINITION('material property','material name',#35147);
#14262=PROPERTY_DEFINITION('material property','density of part',#35147);
#14263=PROPERTY_DEFINITION('material property','material name',#35149);
#14264=PROPERTY_DEFINITION('material property','density of part',#35149);
#14265=PROPERTY_DEFINITION('material property','material name',#35150);
#14266=PROPERTY_DEFINITION('material property','density of part',#35150);
#14267=PROPERTY_DEFINITION('material property','material name',#35151);
#14268=PROPERTY_DEFINITION('material property','density of part',#35151);
#14269=PROPERTY_DEFINITION('material property','material name',#35152);
#14270=PROPERTY_DEFINITION('material property','density of part',#35152);
#14271=PROPERTY_DEFINITION('material property','material name',#35153);
#14272=PROPERTY_DEFINITION('material property','density of part',#35153);
#14273=PROPERTY_DEFINITION('material property','material name',#35154);
#14274=PROPERTY_DEFINITION('material property','density of part',#35154);
#14275=PROPERTY_DEFINITION('material property','material name',#35156);
#14276=PROPERTY_DEFINITION('material property','density of part',#35156);
#14277=PROPERTY_DEFINITION('material property','material name',#35157);
#14278=PROPERTY_DEFINITION('material property','density of part',#35157);
#14279=PROPERTY_DEFINITION('material property','material name',#35159);
#14280=PROPERTY_DEFINITION('material property','density of part',#35159);
#14281=PROPERTY_DEFINITION('material property','material name',#35160);
#14282=PROPERTY_DEFINITION('material property','density of part',#35160);
#14283=PROPERTY_DEFINITION('material property','material name',#35161);
#14284=PROPERTY_DEFINITION('material property','density of part',#35161);
#14285=PROPERTY_DEFINITION('material property','material name',#35162);
#14286=PROPERTY_DEFINITION('material property','density of part',#35162);
#14287=PROPERTY_DEFINITION('material property','material name',#35164);
#14288=PROPERTY_DEFINITION('material property','density of part',#35164);
#14289=PROPERTY_DEFINITION('material property','material name',#35165);
#14290=PROPERTY_DEFINITION('material property','density of part',#35165);
#14291=PROPERTY_DEFINITION('material property','material name',#35166);
#14292=PROPERTY_DEFINITION('material property','density of part',#35166);
#14293=PROPERTY_DEFINITION('material property','material name',#35167);
#14294=PROPERTY_DEFINITION('material property','density of part',#35167);
#14295=PROPERTY_DEFINITION('material property','material name',#35168);
#14296=PROPERTY_DEFINITION('material property','density of part',#35168);
#14297=PROPERTY_DEFINITION('material property','material name',#35169);
#14298=PROPERTY_DEFINITION('material property','density of part',#35169);
#14299=PROPERTY_DEFINITION('material property','material name',#35170);
#14300=PROPERTY_DEFINITION('material property','density of part',#35170);
#14301=PROPERTY_DEFINITION('material property','material name',#35171);
#14302=PROPERTY_DEFINITION('material property','density of part',#35171);
#14303=PROPERTY_DEFINITION('material property','material name',#35172);
#14304=PROPERTY_DEFINITION('material property','density of part',#35172);
#14305=PROPERTY_DEFINITION('material property','material name',#35173);
#14306=PROPERTY_DEFINITION('material property','density of part',#35173);
#14307=PROPERTY_DEFINITION('material property','material name',#35174);
#14308=PROPERTY_DEFINITION('material property','density of part',#35174);
#14309=PROPERTY_DEFINITION('material property','material name',#35175);
#14310=PROPERTY_DEFINITION('material property','density of part',#35175);
#14311=PROPERTY_DEFINITION('material property','material name',#35176);
#14312=PROPERTY_DEFINITION('material property','density of part',#35176);
#14313=PROPERTY_DEFINITION('material property','material name',#35177);
#14314=PROPERTY_DEFINITION('material property','density of part',#35177);
#14315=PROPERTY_DEFINITION('material property','material name',#35179);
#14316=PROPERTY_DEFINITION('material property','density of part',#35179);
#14317=AXIS2_PLACEMENT_3D('',#19457,#15600,#15601);
#14318=AXIS2_PLACEMENT_3D('',#19458,#15602,#15603);
#14319=AXIS2_PLACEMENT_3D('',#19459,#15604,#15605);
#14320=AXIS2_PLACEMENT_3D('',#19460,#15606,#15607);
#14321=AXIS2_PLACEMENT_3D('',#19462,#15608,#15609);
#14322=AXIS2_PLACEMENT_3D('',#19465,#15611,#15612);
#14323=AXIS2_PLACEMENT_3D('',#19466,#15613,#15614);
#14324=AXIS2_PLACEMENT_3D('',#19468,#15615,#15616);
#14325=AXIS2_PLACEMENT_3D('',#19471,#15618,#15619);
#14326=AXIS2_PLACEMENT_3D('',#19472,#15620,#15621);
#14327=AXIS2_PLACEMENT_3D('',#19474,#15622,#15623);
#14328=AXIS2_PLACEMENT_3D('',#19477,#15625,#15626);
#14329=AXIS2_PLACEMENT_3D('',#19478,#15627,#15628);
#14330=AXIS2_PLACEMENT_3D('',#19480,#15629,#15630);
#14331=AXIS2_PLACEMENT_3D('',#19483,#15632,#15633);
#14332=AXIS2_PLACEMENT_3D('',#19484,#15634,#15635);
#14333=AXIS2_PLACEMENT_3D('',#19493,#15640,#15641);
#14334=AXIS2_PLACEMENT_3D('',#19499,#15645,#15646);
#14335=AXIS2_PLACEMENT_3D('',#19505,#15650,#15651);
#14336=AXIS2_PLACEMENT_3D('',#19508,#15654,#15655);
#14337=AXIS2_PLACEMENT_3D('',#19509,#15656,#15657);
#14338=AXIS2_PLACEMENT_3D('',#19510,#15658,#15659);
#14339=AXIS2_PLACEMENT_3D('',#19511,#15660,#15661);
#14340=AXIS2_PLACEMENT_3D('',#19520,#15666,#15667);
#14341=AXIS2_PLACEMENT_3D('',#19526,#15671,#15672);
#14342=AXIS2_PLACEMENT_3D('',#19532,#15676,#15677);
#14343=AXIS2_PLACEMENT_3D('',#19535,#15680,#15681);
#14344=AXIS2_PLACEMENT_3D('',#19536,#15682,#15683);
#14345=AXIS2_PLACEMENT_3D('',#19537,#15684,#15685);
#14346=AXIS2_PLACEMENT_3D('',#19538,#15686,#15687);
#14347=AXIS2_PLACEMENT_3D('',#19547,#15692,#15693);
#14348=AXIS2_PLACEMENT_3D('',#19553,#15697,#15698);
#14349=AXIS2_PLACEMENT_3D('',#19559,#15702,#15703);
#14350=AXIS2_PLACEMENT_3D('',#19562,#15706,#15707);
#14351=AXIS2_PLACEMENT_3D('',#19563,#15708,#15709);
#14352=AXIS2_PLACEMENT_3D('',#19564,#15710,#15711);
#14353=AXIS2_PLACEMENT_3D('',#19565,#15712,#15713);
#14354=AXIS2_PLACEMENT_3D('',#19567,#15714,#15715);
#14355=AXIS2_PLACEMENT_3D('',#19570,#15717,#15718);
#14356=AXIS2_PLACEMENT_3D('',#19571,#15719,#15720);
#14357=AXIS2_PLACEMENT_3D('',#19573,#15721,#15722);
#14358=AXIS2_PLACEMENT_3D('',#19576,#15724,#15725);
#14359=AXIS2_PLACEMENT_3D('',#19577,#15726,#15727);
#14360=AXIS2_PLACEMENT_3D('',#19579,#15728,#15729);
#14361=AXIS2_PLACEMENT_3D('',#19582,#15731,#15732);
#14362=AXIS2_PLACEMENT_3D('',#19583,#15733,#15734);
#14363=AXIS2_PLACEMENT_3D('',#19585,#15735,#15736);
#14364=AXIS2_PLACEMENT_3D('',#19588,#15738,#15739);
#14365=AXIS2_PLACEMENT_3D('',#19589,#15740,#15741);
#14366=AXIS2_PLACEMENT_3D('',#19591,#15742,#15743);
#14367=AXIS2_PLACEMENT_3D('',#19594,#15745,#15746);
#14368=AXIS2_PLACEMENT_3D('',#19595,#15747,#15748);
#14369=AXIS2_PLACEMENT_3D('',#19597,#15749,#15750);
#14370=AXIS2_PLACEMENT_3D('',#19600,#15752,#15753);
#14371=AXIS2_PLACEMENT_3D('',#19601,#15754,#15755);
#14372=AXIS2_PLACEMENT_3D('',#19603,#15756,#15757);
#14373=AXIS2_PLACEMENT_3D('',#19606,#15759,#15760);
#14374=AXIS2_PLACEMENT_3D('',#19607,#15761,#15762);
#14375=AXIS2_PLACEMENT_3D('',#19609,#15763,#15764);
#14376=AXIS2_PLACEMENT_3D('',#19612,#15766,#15767);
#14377=AXIS2_PLACEMENT_3D('',#19613,#15768,#15769);
#14378=AXIS2_PLACEMENT_3D('',#19615,#15770,#15771);
#14379=AXIS2_PLACEMENT_3D('',#19618,#15773,#15774);
#14380=AXIS2_PLACEMENT_3D('',#19619,#15775,#15776);
#14381=AXIS2_PLACEMENT_3D('',#19621,#15777,#15778);
#14382=AXIS2_PLACEMENT_3D('',#19624,#15780,#15781);
#14383=AXIS2_PLACEMENT_3D('',#19625,#15782,#15783);
#14384=AXIS2_PLACEMENT_3D('',#19627,#15784,#15785);
#14385=AXIS2_PLACEMENT_3D('',#19630,#15787,#15788);
#14386=AXIS2_PLACEMENT_3D('',#19631,#15789,#15790);
#14387=AXIS2_PLACEMENT_3D('',#19633,#15791,#15792);
#14388=AXIS2_PLACEMENT_3D('',#19636,#15794,#15795);
#14389=AXIS2_PLACEMENT_3D('',#19637,#15796,#15797);
#14390=AXIS2_PLACEMENT_3D('',#19639,#15798,#15799);
#14391=AXIS2_PLACEMENT_3D('',#19642,#15801,#15802);
#14392=AXIS2_PLACEMENT_3D('',#19643,#15803,#15804);
#14393=AXIS2_PLACEMENT_3D('',#19645,#15805,#15806);
#14394=AXIS2_PLACEMENT_3D('',#19648,#15808,#15809);
#14395=AXIS2_PLACEMENT_3D('',#19649,#15810,#15811);
#14396=AXIS2_PLACEMENT_3D('',#19651,#15812,#15813);
#14397=AXIS2_PLACEMENT_3D('',#19654,#15815,#15816);
#14398=AXIS2_PLACEMENT_3D('',#19655,#15817,#15818);
#14399=AXIS2_PLACEMENT_3D('',#19657,#15819,#15820);
#14400=AXIS2_PLACEMENT_3D('',#19660,#15822,#15823);
#14401=AXIS2_PLACEMENT_3D('',#19661,#15824,#15825);
#14402=AXIS2_PLACEMENT_3D('',#19670,#15830,#15831);
#14403=AXIS2_PLACEMENT_3D('',#19676,#15835,#15836);
#14404=AXIS2_PLACEMENT_3D('',#19682,#15840,#15841);
#14405=AXIS2_PLACEMENT_3D('',#19685,#15844,#15845);
#14406=AXIS2_PLACEMENT_3D('',#19686,#15846,#15847);
#14407=AXIS2_PLACEMENT_3D('',#19687,#15848,#15849);
#14408=AXIS2_PLACEMENT_3D('',#19688,#15850,#15851);
#14409=AXIS2_PLACEMENT_3D('',#19690,#15852,#15853);
#14410=AXIS2_PLACEMENT_3D('',#19693,#15855,#15856);
#14411=AXIS2_PLACEMENT_3D('',#19694,#15857,#15858);
#14412=AXIS2_PLACEMENT_3D('',#19696,#15859,#15860);
#14413=AXIS2_PLACEMENT_3D('',#19697,#15861,#15862);
#14414=AXIS2_PLACEMENT_3D('',#19699,#15863,#15864);
#14415=AXIS2_PLACEMENT_3D('',#19702,#15866,#15867);
#14416=AXIS2_PLACEMENT_3D('',#19703,#15868,#15869);
#14417=AXIS2_PLACEMENT_3D('',#19705,#15870,#15871);
#14418=AXIS2_PLACEMENT_3D('',#19706,#15872,#15873);
#14419=AXIS2_PLACEMENT_3D('',#19708,#15874,#15875);
#14420=AXIS2_PLACEMENT_3D('',#19710,#15877,#15878);
#14421=AXIS2_PLACEMENT_3D('',#19712,#15879,#15880);
#14422=AXIS2_PLACEMENT_3D('',#19714,#15882,#15883);
#14423=AXIS2_PLACEMENT_3D('',#19723,#15888,#15889);
#14424=AXIS2_PLACEMENT_3D('',#19729,#15893,#15894);
#14425=AXIS2_PLACEMENT_3D('',#19735,#15898,#15899);
#14426=AXIS2_PLACEMENT_3D('',#19738,#15902,#15903);
#14427=AXIS2_PLACEMENT_3D('',#19739,#15904,#15905);
#14428=AXIS2_PLACEMENT_3D('',#19740,#15906,#15907);
#14429=AXIS2_PLACEMENT_3D('',#19741,#15908,#15909);
#14430=AXIS2_PLACEMENT_3D('',#19750,#15914,#15915);
#14431=AXIS2_PLACEMENT_3D('',#19756,#15919,#15920);
#14432=AXIS2_PLACEMENT_3D('',#19762,#15924,#15925);
#14433=AXIS2_PLACEMENT_3D('',#19765,#15928,#15929);
#14434=AXIS2_PLACEMENT_3D('',#19766,#15930,#15931);
#14435=AXIS2_PLACEMENT_3D('',#19767,#15932,#15933);
#14436=AXIS2_PLACEMENT_3D('',#19768,#15934,#15935);
#14437=AXIS2_PLACEMENT_3D('',#19770,#15936,#15937);
#14438=AXIS2_PLACEMENT_3D('',#19773,#15939,#15940);
#14439=AXIS2_PLACEMENT_3D('',#19774,#15941,#15942);
#14440=AXIS2_PLACEMENT_3D('',#19776,#15943,#15944);
#14441=AXIS2_PLACEMENT_3D('',#19777,#15945,#15946);
#14442=AXIS2_PLACEMENT_3D('',#19779,#15947,#15948);
#14443=AXIS2_PLACEMENT_3D('',#19782,#15950,#15951);
#14444=AXIS2_PLACEMENT_3D('',#19783,#15952,#15953);
#14445=AXIS2_PLACEMENT_3D('',#19785,#15954,#15955);
#14446=AXIS2_PLACEMENT_3D('',#19786,#15956,#15957);
#14447=AXIS2_PLACEMENT_3D('',#19788,#15958,#15959);
#14448=AXIS2_PLACEMENT_3D('',#19790,#15961,#15962);
#14449=AXIS2_PLACEMENT_3D('',#19792,#15963,#15964);
#14450=AXIS2_PLACEMENT_3D('',#19794,#15966,#15967);
#14451=AXIS2_PLACEMENT_3D('',#19803,#15972,#15973);
#14452=AXIS2_PLACEMENT_3D('',#19809,#15977,#15978);
#14453=AXIS2_PLACEMENT_3D('',#19815,#15982,#15983);
#14454=AXIS2_PLACEMENT_3D('',#19818,#15986,#15987);
#14455=AXIS2_PLACEMENT_3D('',#19819,#15988,#15989);
#14456=AXIS2_PLACEMENT_3D('',#19820,#15990,#15991);
#14457=AXIS2_PLACEMENT_3D('',#19821,#15992,#15993);
#14458=AXIS2_PLACEMENT_3D('',#19830,#15998,#15999);
#14459=AXIS2_PLACEMENT_3D('',#19836,#16003,#16004);
#14460=AXIS2_PLACEMENT_3D('',#19842,#16008,#16009);
#14461=AXIS2_PLACEMENT_3D('',#19845,#16012,#16013);
#14462=AXIS2_PLACEMENT_3D('',#19846,#16014,#16015);
#14463=AXIS2_PLACEMENT_3D('',#19847,#16016,#16017);
#14464=AXIS2_PLACEMENT_3D('',#19848,#16018,#16019);
#14465=AXIS2_PLACEMENT_3D('',#19850,#16020,#16021);
#14466=AXIS2_PLACEMENT_3D('',#19853,#16023,#16024);
#14467=AXIS2_PLACEMENT_3D('',#19854,#16025,#16026);
#14468=AXIS2_PLACEMENT_3D('',#19856,#16027,#16028);
#14469=AXIS2_PLACEMENT_3D('',#19859,#16030,#16031);
#14470=AXIS2_PLACEMENT_3D('',#19860,#16032,#16033);
#14471=AXIS2_PLACEMENT_3D('',#19862,#16034,#16035);
#14472=AXIS2_PLACEMENT_3D('',#19865,#16037,#16038);
#14473=AXIS2_PLACEMENT_3D('',#19866,#16039,#16040);
#14474=AXIS2_PLACEMENT_3D('',#19868,#16041,#16042);
#14475=AXIS2_PLACEMENT_3D('',#19871,#16044,#16045);
#14476=AXIS2_PLACEMENT_3D('',#19872,#16046,#16047);
#14477=AXIS2_PLACEMENT_3D('',#19874,#16048,#16049);
#14478=AXIS2_PLACEMENT_3D('',#19877,#16051,#16052);
#14479=AXIS2_PLACEMENT_3D('',#19878,#16053,#16054);
#14480=AXIS2_PLACEMENT_3D('',#19880,#16055,#16056);
#14481=AXIS2_PLACEMENT_3D('',#19883,#16058,#16059);
#14482=AXIS2_PLACEMENT_3D('',#19884,#16060,#16061);
#14483=AXIS2_PLACEMENT_3D('',#19886,#16062,#16063);
#14484=AXIS2_PLACEMENT_3D('',#19889,#16065,#16066);
#14485=AXIS2_PLACEMENT_3D('',#19890,#16067,#16068);
#14486=AXIS2_PLACEMENT_3D('',#19899,#16073,#16074);
#14487=AXIS2_PLACEMENT_3D('',#19908,#16079,#16080);
#14488=AXIS2_PLACEMENT_3D('',#19914,#16084,#16085);
#14489=AXIS2_PLACEMENT_3D('',#19920,#16089,#16090);
#14490=AXIS2_PLACEMENT_3D('',#19927,#16095,#16096);
#14491=AXIS2_PLACEMENT_3D('',#19931,#16099,#16100);
#14492=AXIS2_PLACEMENT_3D('',#19936,#16104,#16105);
#14493=AXIS2_PLACEMENT_3D('',#19938,#16107,#16108);
#14494=AXIS2_PLACEMENT_3D('',#19939,#16109,#16110);
#14495=AXIS2_PLACEMENT_3D('',#19940,#16111,#16112);
#14496=AXIS2_PLACEMENT_3D('',#19941,#16113,#16114);
#14497=AXIS2_PLACEMENT_3D('',#19943,#16115,#16116);
#14498=AXIS2_PLACEMENT_3D('',#19946,#16118,#16119);
#14499=AXIS2_PLACEMENT_3D('',#19947,#16120,#16121);
#14500=AXIS2_PLACEMENT_3D('',#19949,#16122,#16123);
#14501=AXIS2_PLACEMENT_3D('',#19952,#16125,#16126);
#14502=AXIS2_PLACEMENT_3D('',#19953,#16127,#16128);
#14503=AXIS2_PLACEMENT_3D('',#19955,#16129,#16130);
#14504=AXIS2_PLACEMENT_3D('',#19958,#16132,#16133);
#14505=AXIS2_PLACEMENT_3D('',#19959,#16134,#16135);
#14506=AXIS2_PLACEMENT_3D('',#19961,#16136,#16137);
#14507=AXIS2_PLACEMENT_3D('',#19964,#16139,#16140);
#14508=AXIS2_PLACEMENT_3D('',#19965,#16141,#16142);
#14509=AXIS2_PLACEMENT_3D('',#19967,#16143,#16144);
#14510=AXIS2_PLACEMENT_3D('',#19970,#16146,#16147);
#14511=AXIS2_PLACEMENT_3D('',#19971,#16148,#16149);
#14512=AXIS2_PLACEMENT_3D('',#19973,#16150,#16151);
#14513=AXIS2_PLACEMENT_3D('',#19974,#16152,#16153);
#14514=AXIS2_PLACEMENT_3D('',#19977,#16155,#16156);
#14515=AXIS2_PLACEMENT_3D('',#19978,#16157,#16158);
#14516=AXIS2_PLACEMENT_3D('',#19980,#16159,#16160);
#14517=AXIS2_PLACEMENT_3D('',#19983,#16162,#16163);
#14518=AXIS2_PLACEMENT_3D('',#19984,#16164,#16165);
#14519=AXIS2_PLACEMENT_3D('',#19985,#16166,#16167);
#14520=AXIS2_PLACEMENT_3D('',#19986,#16168,#16169);
#14521=AXIS2_PLACEMENT_3D('',#19987,#16170,#16171);
#14522=AXIS2_PLACEMENT_3D('',#19989,#16172,#16173);
#14523=AXIS2_PLACEMENT_3D('',#19992,#16175,#16176);
#14524=AXIS2_PLACEMENT_3D('',#19993,#16177,#16178);
#14525=AXIS2_PLACEMENT_3D('',#19995,#16179,#16180);
#14526=AXIS2_PLACEMENT_3D('',#19998,#16182,#16183);
#14527=AXIS2_PLACEMENT_3D('',#19999,#16184,#16185);
#14528=AXIS2_PLACEMENT_3D('',#20001,#16186,#16187);
#14529=AXIS2_PLACEMENT_3D('',#20004,#16189,#16190);
#14530=AXIS2_PLACEMENT_3D('',#20005,#16191,#16192);
#14531=AXIS2_PLACEMENT_3D('',#20007,#16193,#16194);
#14532=AXIS2_PLACEMENT_3D('',#20010,#16196,#16197);
#14533=AXIS2_PLACEMENT_3D('',#20011,#16198,#16199);
#14534=AXIS2_PLACEMENT_3D('',#20013,#16200,#16201);
#14535=AXIS2_PLACEMENT_3D('',#20016,#16203,#16204);
#14536=AXIS2_PLACEMENT_3D('',#20017,#16205,#16206);
#14537=AXIS2_PLACEMENT_3D('',#20019,#16207,#16208);
#14538=AXIS2_PLACEMENT_3D('',#20020,#16209,#16210);
#14539=AXIS2_PLACEMENT_3D('',#20022,#16211,#16212);
#14540=AXIS2_PLACEMENT_3D('',#20024,#16214,#16215);
#14541=AXIS2_PLACEMENT_3D('',#20026,#16216,#16217);
#14542=AXIS2_PLACEMENT_3D('',#20029,#16219,#16220);
#14543=AXIS2_PLACEMENT_3D('',#20030,#16221,#16222);
#14544=AXIS2_PLACEMENT_3D('',#20031,#16223,#16224);
#14545=AXIS2_PLACEMENT_3D('',#20032,#16225,#16226);
#14546=AXIS2_PLACEMENT_3D('',#20033,#16227,#16228);
#14547=AXIS2_PLACEMENT_3D('',#20035,#16229,#16230);
#14548=AXIS2_PLACEMENT_3D('',#20038,#16232,#16233);
#14549=AXIS2_PLACEMENT_3D('',#20039,#16234,#16235);
#14550=AXIS2_PLACEMENT_3D('',#20041,#16236,#16237);
#14551=AXIS2_PLACEMENT_3D('',#20044,#16239,#16240);
#14552=AXIS2_PLACEMENT_3D('',#20045,#16241,#16242);
#14553=AXIS2_PLACEMENT_3D('',#20047,#16243,#16244);
#14554=AXIS2_PLACEMENT_3D('',#20050,#16246,#16247);
#14555=AXIS2_PLACEMENT_3D('',#20051,#16248,#16249);
#14556=AXIS2_PLACEMENT_3D('',#20053,#16250,#16251);
#14557=AXIS2_PLACEMENT_3D('',#20056,#16253,#16254);
#14558=AXIS2_PLACEMENT_3D('',#20057,#16255,#16256);
#14559=AXIS2_PLACEMENT_3D('',#20059,#16257,#16258);
#14560=AXIS2_PLACEMENT_3D('',#20062,#16260,#16261);
#14561=AXIS2_PLACEMENT_3D('',#20063,#16262,#16263);
#14562=AXIS2_PLACEMENT_3D('',#20065,#16264,#16265);
#14563=AXIS2_PLACEMENT_3D('',#20068,#16267,#16268);
#14564=AXIS2_PLACEMENT_3D('',#20069,#16269,#16270);
#14565=AXIS2_PLACEMENT_3D('',#20071,#16271,#16272);
#14566=AXIS2_PLACEMENT_3D('',#20074,#16274,#16275);
#14567=AXIS2_PLACEMENT_3D('',#20075,#16276,#16277);
#14568=AXIS2_PLACEMENT_3D('',#20084,#16282,#16283);
#14569=AXIS2_PLACEMENT_3D('',#20093,#16288,#16289);
#14570=AXIS2_PLACEMENT_3D('',#20099,#16293,#16294);
#14571=AXIS2_PLACEMENT_3D('',#20105,#16298,#16299);
#14572=AXIS2_PLACEMENT_3D('',#20112,#16304,#16305);
#14573=AXIS2_PLACEMENT_3D('',#20116,#16308,#16309);
#14574=AXIS2_PLACEMENT_3D('',#20121,#16313,#16314);
#14575=AXIS2_PLACEMENT_3D('',#20123,#16316,#16317);
#14576=AXIS2_PLACEMENT_3D('',#20124,#16318,#16319);
#14577=AXIS2_PLACEMENT_3D('',#20125,#16320,#16321);
#14578=AXIS2_PLACEMENT_3D('',#20126,#16322,#16323);
#14579=AXIS2_PLACEMENT_3D('',#20128,#16324,#16325);
#14580=AXIS2_PLACEMENT_3D('',#20131,#16327,#16328);
#14581=AXIS2_PLACEMENT_3D('',#20132,#16329,#16330);
#14582=AXIS2_PLACEMENT_3D('',#20134,#16331,#16332);
#14583=AXIS2_PLACEMENT_3D('',#20137,#16334,#16335);
#14584=AXIS2_PLACEMENT_3D('',#20138,#16336,#16337);
#14585=AXIS2_PLACEMENT_3D('',#20140,#16338,#16339);
#14586=AXIS2_PLACEMENT_3D('',#20143,#16341,#16342);
#14587=AXIS2_PLACEMENT_3D('',#20144,#16343,#16344);
#14588=AXIS2_PLACEMENT_3D('',#20146,#16345,#16346);
#14589=AXIS2_PLACEMENT_3D('',#20149,#16348,#16349);
#14590=AXIS2_PLACEMENT_3D('',#20150,#16350,#16351);
#14591=AXIS2_PLACEMENT_3D('',#20152,#16352,#16353);
#14592=AXIS2_PLACEMENT_3D('',#20155,#16355,#16356);
#14593=AXIS2_PLACEMENT_3D('',#20156,#16357,#16358);
#14594=AXIS2_PLACEMENT_3D('',#20158,#16359,#16360);
#14595=AXIS2_PLACEMENT_3D('',#20159,#16361,#16362);
#14596=AXIS2_PLACEMENT_3D('',#20162,#16364,#16365);
#14597=AXIS2_PLACEMENT_3D('',#20163,#16366,#16367);
#14598=AXIS2_PLACEMENT_3D('',#20165,#16368,#16369);
#14599=AXIS2_PLACEMENT_3D('',#20168,#16371,#16372);
#14600=AXIS2_PLACEMENT_3D('',#20169,#16373,#16374);
#14601=AXIS2_PLACEMENT_3D('',#20170,#16375,#16376);
#14602=AXIS2_PLACEMENT_3D('',#20171,#16377,#16378);
#14603=AXIS2_PLACEMENT_3D('',#20172,#16379,#16380);
#14604=AXIS2_PLACEMENT_3D('',#20174,#16381,#16382);
#14605=AXIS2_PLACEMENT_3D('',#20177,#16384,#16385);
#14606=AXIS2_PLACEMENT_3D('',#20178,#16386,#16387);
#14607=AXIS2_PLACEMENT_3D('',#20180,#16388,#16389);
#14608=AXIS2_PLACEMENT_3D('',#20183,#16391,#16392);
#14609=AXIS2_PLACEMENT_3D('',#20184,#16393,#16394);
#14610=AXIS2_PLACEMENT_3D('',#20186,#16395,#16396);
#14611=AXIS2_PLACEMENT_3D('',#20189,#16398,#16399);
#14612=AXIS2_PLACEMENT_3D('',#20190,#16400,#16401);
#14613=AXIS2_PLACEMENT_3D('',#20192,#16402,#16403);
#14614=AXIS2_PLACEMENT_3D('',#20195,#16405,#16406);
#14615=AXIS2_PLACEMENT_3D('',#20196,#16407,#16408);
#14616=AXIS2_PLACEMENT_3D('',#20198,#16409,#16410);
#14617=AXIS2_PLACEMENT_3D('',#20201,#16412,#16413);
#14618=AXIS2_PLACEMENT_3D('',#20202,#16414,#16415);
#14619=AXIS2_PLACEMENT_3D('',#20204,#16416,#16417);
#14620=AXIS2_PLACEMENT_3D('',#20205,#16418,#16419);
#14621=AXIS2_PLACEMENT_3D('',#20207,#16420,#16421);
#14622=AXIS2_PLACEMENT_3D('',#20209,#16423,#16424);
#14623=AXIS2_PLACEMENT_3D('',#20211,#16425,#16426);
#14624=AXIS2_PLACEMENT_3D('',#20214,#16428,#16429);
#14625=AXIS2_PLACEMENT_3D('',#20215,#16430,#16431);
#14626=AXIS2_PLACEMENT_3D('',#20216,#16432,#16433);
#14627=AXIS2_PLACEMENT_3D('',#20217,#16434,#16435);
#14628=AXIS2_PLACEMENT_3D('',#20218,#16436,#16437);
#14629=AXIS2_PLACEMENT_3D('',#20227,#16442,#16443);
#14630=AXIS2_PLACEMENT_3D('',#20233,#16447,#16448);
#14631=AXIS2_PLACEMENT_3D('',#20239,#16452,#16453);
#14632=AXIS2_PLACEMENT_3D('',#20245,#16457,#16458);
#14633=AXIS2_PLACEMENT_3D('',#20251,#16462,#16463);
#14634=AXIS2_PLACEMENT_3D('',#20257,#16467,#16468);
#14635=AXIS2_PLACEMENT_3D('',#20263,#16472,#16473);
#14636=AXIS2_PLACEMENT_3D('',#20269,#16477,#16478);
#14637=AXIS2_PLACEMENT_3D('',#20275,#16482,#16483);
#14638=AXIS2_PLACEMENT_3D('',#20284,#16488,#16489);
#14639=AXIS2_PLACEMENT_3D('',#20290,#16493,#16494);
#14640=AXIS2_PLACEMENT_3D('',#20296,#16498,#16499);
#14641=AXIS2_PLACEMENT_3D('',#20302,#16503,#16504);
#14642=AXIS2_PLACEMENT_3D('',#20308,#16508,#16509);
#14643=AXIS2_PLACEMENT_3D('',#20314,#16513,#16514);
#14644=AXIS2_PLACEMENT_3D('',#20320,#16518,#16519);
#14645=AXIS2_PLACEMENT_3D('',#20326,#16523,#16524);
#14646=AXIS2_PLACEMENT_3D('',#20332,#16528,#16529);
#14647=AXIS2_PLACEMENT_3D('',#20341,#16534,#16535);
#14648=AXIS2_PLACEMENT_3D('',#20347,#16539,#16540);
#14649=AXIS2_PLACEMENT_3D('',#20353,#16544,#16545);
#14650=AXIS2_PLACEMENT_3D('',#20359,#16549,#16550);
#14651=AXIS2_PLACEMENT_3D('',#20365,#16554,#16555);
#14652=AXIS2_PLACEMENT_3D('',#20371,#16559,#16560);
#14653=AXIS2_PLACEMENT_3D('',#20377,#16564,#16565);
#14654=AXIS2_PLACEMENT_3D('',#20383,#16569,#16570);
#14655=AXIS2_PLACEMENT_3D('',#20389,#16574,#16575);
#14656=AXIS2_PLACEMENT_3D('',#20398,#16580,#16581);
#14657=AXIS2_PLACEMENT_3D('',#20404,#16585,#16586);
#14658=AXIS2_PLACEMENT_3D('',#20410,#16590,#16591);
#14659=AXIS2_PLACEMENT_3D('',#20416,#16595,#16596);
#14660=AXIS2_PLACEMENT_3D('',#20422,#16600,#16601);
#14661=AXIS2_PLACEMENT_3D('',#20428,#16605,#16606);
#14662=AXIS2_PLACEMENT_3D('',#20434,#16610,#16611);
#14663=AXIS2_PLACEMENT_3D('',#20440,#16615,#16616);
#14664=AXIS2_PLACEMENT_3D('',#20446,#16620,#16621);
#14665=AXIS2_PLACEMENT_3D('',#20448,#16622,#16623);
#14666=AXIS2_PLACEMENT_3D('',#20451,#16625,#16626);
#14667=AXIS2_PLACEMENT_3D('',#20452,#16627,#16628);
#14668=AXIS2_PLACEMENT_3D('',#20458,#16632,#16633);
#14669=AXIS2_PLACEMENT_3D('',#20464,#16637,#16638);
#14670=AXIS2_PLACEMENT_3D('',#20467,#16641,#16642);
#14671=AXIS2_PLACEMENT_3D('',#20473,#16646,#16647);
#14672=AXIS2_PLACEMENT_3D('',#20476,#16650,#16651);
#14673=AXIS2_PLACEMENT_3D('',#20482,#16655,#16656);
#14674=AXIS2_PLACEMENT_3D('',#20485,#16659,#16660);
#14675=AXIS2_PLACEMENT_3D('',#20488,#16663,#16664);
#14676=AXIS2_PLACEMENT_3D('',#20489,#16665,#16666);
#14677=AXIS2_PLACEMENT_3D('',#20490,#16667,#16668);
#14678=AXIS2_PLACEMENT_3D('',#20491,#16669,#16670);
#14679=AXIS2_PLACEMENT_3D('',#20500,#16675,#16676);
#14680=AXIS2_PLACEMENT_3D('',#20506,#16680,#16681);
#14681=AXIS2_PLACEMENT_3D('',#20513,#16685,#16686);
#14682=AXIS2_PLACEMENT_3D('',#20514,#16687,#16688);
#14683=AXIS2_PLACEMENT_3D('',#20528,#16696,#16697);
#14684=AXIS2_PLACEMENT_3D('',#20532,#16700,#16701);
#14685=AXIS2_PLACEMENT_3D('',#20536,#16704,#16705);
#14686=AXIS2_PLACEMENT_3D('',#20546,#16711,#16712);
#14687=AXIS2_PLACEMENT_3D('',#20548,#16714,#16715);
#14688=AXIS2_PLACEMENT_3D('',#20552,#16717,#16718);
#14689=AXIS2_PLACEMENT_3D('',#20554,#16720,#16721);
#14690=AXIS2_PLACEMENT_3D('',#20556,#16722,#16723);
#14691=AXIS2_PLACEMENT_3D('',#20559,#16725,#16726);
#14692=AXIS2_PLACEMENT_3D('',#20561,#16727,#16728);
#14693=AXIS2_PLACEMENT_3D('',#20562,#16729,#16730);
#14694=AXIS2_PLACEMENT_3D('',#20563,#16731,#16732);
#14695=AXIS2_PLACEMENT_3D('',#20565,#16734,#16735);
#14696=AXIS2_PLACEMENT_3D('',#20567,#16737,#16738);
#14697=AXIS2_PLACEMENT_3D('',#20569,#16740,#16741);
#14698=AXIS2_PLACEMENT_3D('',#20570,#16742,#16743);
#14699=AXIS2_PLACEMENT_3D('',#20571,#16744,#16745);
#14700=AXIS2_PLACEMENT_3D('',#20573,#16746,#16747);
#14701=AXIS2_PLACEMENT_3D('',#20576,#16749,#16750);
#14702=AXIS2_PLACEMENT_3D('',#20577,#16751,#16752);
#14703=AXIS2_PLACEMENT_3D('',#20580,#16754,#16755);
#14704=AXIS2_PLACEMENT_3D('',#20581,#16756,#16757);
#14705=AXIS2_PLACEMENT_3D('',#20583,#16758,#16759);
#14706=AXIS2_PLACEMENT_3D('',#20584,#16760,#16761);
#14707=AXIS2_PLACEMENT_3D('',#20587,#16763,#16764);
#14708=AXIS2_PLACEMENT_3D('',#20588,#16765,#16766);
#14709=AXIS2_PLACEMENT_3D('',#20589,#16767,#16768);
#14710=AXIS2_PLACEMENT_3D('',#20590,#16769,#16770);
#14711=AXIS2_PLACEMENT_3D('',#20592,#16771,#16772);
#14712=AXIS2_PLACEMENT_3D('',#20595,#16774,#16775);
#14713=AXIS2_PLACEMENT_3D('',#20596,#16776,#16777);
#14714=AXIS2_PLACEMENT_3D('',#20598,#16778,#16779);
#14715=AXIS2_PLACEMENT_3D('',#20599,#16780,#16781);
#14716=AXIS2_PLACEMENT_3D('',#20601,#16782,#16783);
#14717=AXIS2_PLACEMENT_3D('',#20604,#16785,#16786);
#14718=AXIS2_PLACEMENT_3D('',#20605,#16787,#16788);
#14719=AXIS2_PLACEMENT_3D('',#20607,#16789,#16790);
#14720=AXIS2_PLACEMENT_3D('',#20608,#16791,#16792);
#14721=AXIS2_PLACEMENT_3D('',#20610,#16793,#16794);
#14722=AXIS2_PLACEMENT_3D('',#20613,#16796,#16797);
#14723=AXIS2_PLACEMENT_3D('',#20614,#16798,#16799);
#14724=AXIS2_PLACEMENT_3D('',#20616,#16800,#16801);
#14725=AXIS2_PLACEMENT_3D('',#20617,#16802,#16803);
#14726=AXIS2_PLACEMENT_3D('',#20619,#16804,#16805);
#14727=AXIS2_PLACEMENT_3D('',#20622,#16807,#16808);
#14728=AXIS2_PLACEMENT_3D('',#20623,#16809,#16810);
#14729=AXIS2_PLACEMENT_3D('',#20625,#16811,#16812);
#14730=AXIS2_PLACEMENT_3D('',#20626,#16813,#16814);
#14731=AXIS2_PLACEMENT_3D('',#20628,#16815,#16816);
#14732=AXIS2_PLACEMENT_3D('',#20630,#16818,#16819);
#14733=AXIS2_PLACEMENT_3D('',#20632,#16820,#16821);
#14734=AXIS2_PLACEMENT_3D('',#20634,#16823,#16824);
#14735=AXIS2_PLACEMENT_3D('',#20636,#16825,#16826);
#14736=AXIS2_PLACEMENT_3D('',#20638,#16828,#16829);
#14737=AXIS2_PLACEMENT_3D('',#20640,#16830,#16831);
#14738=AXIS2_PLACEMENT_3D('',#20642,#16833,#16834);
#14739=AXIS2_PLACEMENT_3D('',#20651,#16839,#16840);
#14740=AXIS2_PLACEMENT_3D('',#20657,#16844,#16845);
#14741=AXIS2_PLACEMENT_3D('',#20663,#16849,#16850);
#14742=AXIS2_PLACEMENT_3D('',#20669,#16854,#16855);
#14743=AXIS2_PLACEMENT_3D('',#20675,#16859,#16860);
#14744=AXIS2_PLACEMENT_3D('',#20681,#16864,#16865);
#14745=AXIS2_PLACEMENT_3D('',#20687,#16869,#16870);
#14746=AXIS2_PLACEMENT_3D('',#20693,#16874,#16875);
#14747=AXIS2_PLACEMENT_3D('',#20699,#16879,#16880);
#14748=AXIS2_PLACEMENT_3D('',#20705,#16884,#16885);
#14749=AXIS2_PLACEMENT_3D('',#20711,#16889,#16890);
#14750=AXIS2_PLACEMENT_3D('',#20714,#16893,#16894);
#14751=AXIS2_PLACEMENT_3D('',#20715,#16895,#16896);
#14752=AXIS2_PLACEMENT_3D('',#20716,#16897,#16898);
#14753=AXIS2_PLACEMENT_3D('',#20717,#16899,#16900);
#14754=AXIS2_PLACEMENT_3D('',#20719,#16901,#16902);
#14755=AXIS2_PLACEMENT_3D('',#20720,#16903,#16904);
#14756=AXIS2_PLACEMENT_3D('',#20722,#16905,#16906);
#14757=AXIS2_PLACEMENT_3D('',#20724,#16908,#16909);
#14758=AXIS2_PLACEMENT_3D('',#20726,#16910,#16911);
#14759=AXIS2_PLACEMENT_3D('',#20728,#16913,#16914);
#14760=AXIS2_PLACEMENT_3D('',#20730,#16915,#16916);
#14761=AXIS2_PLACEMENT_3D('',#20732,#16918,#16919);
#14762=AXIS2_PLACEMENT_3D('',#20734,#16920,#16921);
#14763=AXIS2_PLACEMENT_3D('',#20735,#16922,#16923);
#14764=AXIS2_PLACEMENT_3D('',#20737,#16924,#16925);
#14765=AXIS2_PLACEMENT_3D('',#20739,#16927,#16928);
#14766=AXIS2_PLACEMENT_3D('',#20741,#16929,#16930);
#14767=AXIS2_PLACEMENT_3D('',#20743,#16932,#16933);
#14768=AXIS2_PLACEMENT_3D('',#20745,#16934,#16935);
#14769=AXIS2_PLACEMENT_3D('',#20747,#16937,#16938);
#14770=AXIS2_PLACEMENT_3D('',#20748,#16939,#16940);
#14771=AXIS2_PLACEMENT_3D('',#20757,#16945,#16946);
#14772=AXIS2_PLACEMENT_3D('',#20763,#16950,#16951);
#14773=AXIS2_PLACEMENT_3D('',#20769,#16955,#16956);
#14774=AXIS2_PLACEMENT_3D('',#20775,#16960,#16961);
#14775=AXIS2_PLACEMENT_3D('',#20781,#16965,#16966);
#14776=AXIS2_PLACEMENT_3D('',#20784,#16969,#16970);
#14777=AXIS2_PLACEMENT_3D('',#20785,#16971,#16972);
#14778=AXIS2_PLACEMENT_3D('',#20786,#16973,#16974);
#14779=AXIS2_PLACEMENT_3D('',#20787,#16975,#16976);
#14780=AXIS2_PLACEMENT_3D('',#20788,#16977,#16978);
#14781=AXIS2_PLACEMENT_3D('',#20791,#16979,#16980);
#14782=AXIS2_PLACEMENT_3D('',#20792,#16981,#16982);
#14783=AXIS2_PLACEMENT_3D('',#20794,#16983,#16984);
#14784=AXIS2_PLACEMENT_3D('',#20796,#16985,#16986);
#14785=AXIS2_PLACEMENT_3D('',#20797,#16987,#16988);
#14786=AXIS2_PLACEMENT_3D('',#20798,#16989,#16990);
#14787=AXIS2_PLACEMENT_3D('',#20801,#16992,#16993);
#14788=AXIS2_PLACEMENT_3D('',#20802,#16994,#16995);
#14789=AXIS2_PLACEMENT_3D('',#20804,#16996,#16997);
#14790=AXIS2_PLACEMENT_3D('',#20807,#16999,#17000);
#14791=AXIS2_PLACEMENT_3D('',#20808,#17001,#17002);
#14792=AXIS2_PLACEMENT_3D('',#20811,#17004,#17005);
#14793=AXIS2_PLACEMENT_3D('',#20812,#17006,#17007);
#14794=AXIS2_PLACEMENT_3D('',#20813,#17008,#17009);
#14795=AXIS2_PLACEMENT_3D('',#20815,#17010,#17011);
#14796=AXIS2_PLACEMENT_3D('',#20817,#17013,#17014);
#14797=AXIS2_PLACEMENT_3D('',#20819,#17015,#17016);
#14798=AXIS2_PLACEMENT_3D('',#20820,#17017,#17018);
#14799=AXIS2_PLACEMENT_3D('',#20822,#17020,#17021);
#14800=AXIS2_PLACEMENT_3D('',#20823,#17022,#17023);
#14801=AXIS2_PLACEMENT_3D('',#20826,#17024,#17025);
#14802=AXIS2_PLACEMENT_3D('',#20827,#17026,#17027);
#14803=AXIS2_PLACEMENT_3D('',#20829,#17028,#17029);
#14804=AXIS2_PLACEMENT_3D('',#20831,#17030,#17031);
#14805=AXIS2_PLACEMENT_3D('',#20832,#17032,#17033);
#14806=AXIS2_PLACEMENT_3D('',#20833,#17034,#17035);
#14807=AXIS2_PLACEMENT_3D('',#20835,#17036,#17037);
#14808=AXIS2_PLACEMENT_3D('',#20837,#17039,#17040);
#14809=AXIS2_PLACEMENT_3D('',#20839,#17041,#17042);
#14810=AXIS2_PLACEMENT_3D('',#20841,#17043,#17044);
#14811=AXIS2_PLACEMENT_3D('',#20842,#17045,#17046);
#14812=AXIS2_PLACEMENT_3D('',#20844,#17047,#17048);
#14813=AXIS2_PLACEMENT_3D('',#20846,#17050,#17051);
#14814=AXIS2_PLACEMENT_3D('',#20848,#17052,#17053);
#14815=AXIS2_PLACEMENT_3D('',#20850,#17055,#17056);
#14816=AXIS2_PLACEMENT_3D('',#20852,#17057,#17058);
#14817=AXIS2_PLACEMENT_3D('',#20854,#17060,#17061);
#14818=AXIS2_PLACEMENT_3D('',#20855,#17062,#17063);
#14819=AXIS2_PLACEMENT_3D('',#20857,#17065,#17066);
#14820=AXIS2_PLACEMENT_3D('',#20858,#17067,#17068);
#14821=AXIS2_PLACEMENT_3D('',#20861,#17069,#17070);
#14822=AXIS2_PLACEMENT_3D('',#20862,#17071,#17072);
#14823=AXIS2_PLACEMENT_3D('',#20865,#17073,#17074);
#14824=AXIS2_PLACEMENT_3D('',#20866,#17075,#17076);
#14825=AXIS2_PLACEMENT_3D('',#20869,#17077,#17078);
#14826=AXIS2_PLACEMENT_3D('',#20870,#17079,#17080);
#14827=AXIS2_PLACEMENT_3D('',#20873,#17081,#17082);
#14828=AXIS2_PLACEMENT_3D('',#20874,#17083,#17084);
#14829=AXIS2_PLACEMENT_3D('',#20877,#17085,#17086);
#14830=AXIS2_PLACEMENT_3D('',#20878,#17087,#17088);
#14831=AXIS2_PLACEMENT_3D('',#20881,#17089,#17090);
#14832=AXIS2_PLACEMENT_3D('',#20882,#17091,#17092);
#14833=AXIS2_PLACEMENT_3D('',#20885,#17093,#17094);
#14834=AXIS2_PLACEMENT_3D('',#20886,#17095,#17096);
#14835=AXIS2_PLACEMENT_3D('',#20887,#17097,#17098);
#14836=AXIS2_PLACEMENT_3D('',#20913,#17099,#17100);
#14837=AXIS2_PLACEMENT_3D('',#20937,#17101,#17102);
#14838=AXIS2_PLACEMENT_3D('',#20938,#17103,#17104);
#14839=AXIS2_PLACEMENT_3D('',#20940,#17105,#17106);
#14840=AXIS2_PLACEMENT_3D('',#20965,#17107,#17108);
#14841=AXIS2_PLACEMENT_3D('',#20990,#17109,#17110);
#14842=AXIS2_PLACEMENT_3D('',#20993,#17112,#17113);
#14843=AXIS2_PLACEMENT_3D('',#20995,#17114,#17115);
#14844=AXIS2_PLACEMENT_3D('',#21020,#17116,#17117);
#14845=AXIS2_PLACEMENT_3D('',#21045,#17118,#17119);
#14846=AXIS2_PLACEMENT_3D('',#21070,#17120,#17121);
#14847=AXIS2_PLACEMENT_3D('',#21094,#17122,#17123);
#14848=AXIS2_PLACEMENT_3D('',#21095,#17124,#17125);
#14849=AXIS2_PLACEMENT_3D('',#21097,#17126,#17127);
#14850=AXIS2_PLACEMENT_3D('',#21098,#17128,#17129);
#14851=AXIS2_PLACEMENT_3D('',#21099,#17130,#17131);
#14852=AXIS2_PLACEMENT_3D('',#21123,#17132,#17133);
#14853=AXIS2_PLACEMENT_3D('',#21124,#17134,#17135);
#14854=AXIS2_PLACEMENT_3D('',#21126,#17136,#17137);
#14855=AXIS2_PLACEMENT_3D('',#21127,#17138,#17139);
#14856=AXIS2_PLACEMENT_3D('',#21128,#17140,#17141);
#14857=AXIS2_PLACEMENT_3D('',#21152,#17142,#17143);
#14858=AXIS2_PLACEMENT_3D('',#21153,#17144,#17145);
#14859=AXIS2_PLACEMENT_3D('',#21155,#17146,#17147);
#14860=AXIS2_PLACEMENT_3D('',#21157,#17148,#17149);
#14861=AXIS2_PLACEMENT_3D('',#21158,#17150,#17151);
#14862=AXIS2_PLACEMENT_3D('',#21159,#17152,#17153);
#14863=AXIS2_PLACEMENT_3D('',#21183,#17154,#17155);
#14864=AXIS2_PLACEMENT_3D('',#21184,#17156,#17157);
#14865=AXIS2_PLACEMENT_3D('',#21186,#17158,#17159);
#14866=AXIS2_PLACEMENT_3D('',#21187,#17160,#17161);
#14867=AXIS2_PLACEMENT_3D('',#21188,#17162,#17163);
#14868=AXIS2_PLACEMENT_3D('',#21212,#17164,#17165);
#14869=AXIS2_PLACEMENT_3D('',#21213,#17166,#17167);
#14870=AXIS2_PLACEMENT_3D('',#21215,#17168,#17169);
#14871=AXIS2_PLACEMENT_3D('',#21216,#17170,#17171);
#14872=AXIS2_PLACEMENT_3D('',#21217,#17172,#17173);
#14873=AXIS2_PLACEMENT_3D('',#21241,#17174,#17175);
#14874=AXIS2_PLACEMENT_3D('',#21242,#17176,#17177);
#14875=AXIS2_PLACEMENT_3D('',#21244,#17178,#17179);
#14876=AXIS2_PLACEMENT_3D('',#21247,#17181,#17182);
#14877=AXIS2_PLACEMENT_3D('',#21271,#17183,#17184);
#14878=AXIS2_PLACEMENT_3D('',#21272,#17185,#17186);
#14879=AXIS2_PLACEMENT_3D('',#21273,#17187,#17188);
#14880=AXIS2_PLACEMENT_3D('',#21274,#17189,#17190);
#14881=AXIS2_PLACEMENT_3D('',#21275,#17191,#17192);
#14882=AXIS2_PLACEMENT_3D('',#21276,#17193,#17194);
#14883=AXIS2_PLACEMENT_3D('',#21277,#17195,#17196);
#14884=AXIS2_PLACEMENT_3D('',#21278,#17197,#17198);
#14885=AXIS2_PLACEMENT_3D('',#21279,#17199,#17200);
#14886=AXIS2_PLACEMENT_3D('',#21281,#17201,#17202);
#14887=AXIS2_PLACEMENT_3D('',#21283,#17203,#17204);
#14888=AXIS2_PLACEMENT_3D('',#21284,#17205,#17206);
#14889=AXIS2_PLACEMENT_3D('',#21286,#17207,#17208);
#14890=AXIS2_PLACEMENT_3D('',#21288,#17210,#17211);
#14891=AXIS2_PLACEMENT_3D('',#21290,#17212,#17213);
#14892=AXIS2_PLACEMENT_3D('',#21291,#17214,#17215);
#14893=AXIS2_PLACEMENT_3D('',#21293,#17217,#17218);
#14894=AXIS2_PLACEMENT_3D('',#21295,#17219,#17220);
#14895=AXIS2_PLACEMENT_3D('',#21297,#17221,#17222);
#14896=AXIS2_PLACEMENT_3D('',#21298,#17223,#17224);
#14897=AXIS2_PLACEMENT_3D('',#21300,#17225,#17226);
#14898=AXIS2_PLACEMENT_3D('',#21302,#17228,#17229);
#14899=AXIS2_PLACEMENT_3D('',#21304,#17230,#17231);
#14900=AXIS2_PLACEMENT_3D('',#21305,#17232,#17233);
#14901=AXIS2_PLACEMENT_3D('',#21307,#17235,#17236);
#14902=AXIS2_PLACEMENT_3D('',#21308,#17237,#17238);
#14903=AXIS2_PLACEMENT_3D('',#21309,#17239,#17240);
#14904=AXIS2_PLACEMENT_3D('',#21310,#17241,#17242);
#14905=AXIS2_PLACEMENT_3D('',#21311,#17243,#17244);
#14906=AXIS2_PLACEMENT_3D('',#21312,#17245,#17246);
#14907=AXIS2_PLACEMENT_3D('',#21313,#17247,#17248);
#14908=AXIS2_PLACEMENT_3D('',#21322,#17253,#17254);
#14909=AXIS2_PLACEMENT_3D('',#21328,#17258,#17259);
#14910=AXIS2_PLACEMENT_3D('',#21334,#17263,#17264);
#14911=AXIS2_PLACEMENT_3D('',#21340,#17268,#17269);
#14912=AXIS2_PLACEMENT_3D('',#21346,#17273,#17274);
#14913=AXIS2_PLACEMENT_3D('',#21349,#17277,#17278);
#14914=AXIS2_PLACEMENT_3D('',#21350,#17279,#17280);
#14915=AXIS2_PLACEMENT_3D('',#21351,#17281,#17282);
#14916=AXIS2_PLACEMENT_3D('',#21353,#17283,#17284);
#14917=AXIS2_PLACEMENT_3D('',#21354,#17285,#17286);
#14918=AXIS2_PLACEMENT_3D('',#21356,#17287,#17288);
#14919=AXIS2_PLACEMENT_3D('',#21357,#17289,#17290);
#14920=AXIS2_PLACEMENT_3D('',#21359,#17291,#17292);
#14921=AXIS2_PLACEMENT_3D('',#21361,#17294,#17295);
#14922=AXIS2_PLACEMENT_3D('',#21363,#17296,#17297);
#14923=AXIS2_PLACEMENT_3D('',#21365,#17299,#17300);
#14924=AXIS2_PLACEMENT_3D('',#21367,#17301,#17302);
#14925=AXIS2_PLACEMENT_3D('',#21369,#17304,#17305);
#14926=AXIS2_PLACEMENT_3D('',#21371,#17306,#17307);
#14927=AXIS2_PLACEMENT_3D('',#21372,#17308,#17309);
#14928=AXIS2_PLACEMENT_3D('',#21374,#17310,#17311);
#14929=AXIS2_PLACEMENT_3D('',#21376,#17313,#17314);
#14930=AXIS2_PLACEMENT_3D('',#21378,#17316,#17317);
#14931=AXIS2_PLACEMENT_3D('',#21379,#17318,#17319);
#14932=AXIS2_PLACEMENT_3D('',#21380,#17320,#17321);
#14933=AXIS2_PLACEMENT_3D('',#21382,#17322,#17323);
#14934=AXIS2_PLACEMENT_3D('',#21385,#17325,#17326);
#14935=AXIS2_PLACEMENT_3D('',#21386,#17327,#17328);
#14936=AXIS2_PLACEMENT_3D('',#21388,#17329,#17330);
#14937=AXIS2_PLACEMENT_3D('',#21391,#17332,#17333);
#14938=AXIS2_PLACEMENT_3D('',#21392,#17334,#17335);
#14939=AXIS2_PLACEMENT_3D('',#21394,#17336,#17337);
#14940=AXIS2_PLACEMENT_3D('',#21397,#17339,#17340);
#14941=AXIS2_PLACEMENT_3D('',#21398,#17341,#17342);
#14942=AXIS2_PLACEMENT_3D('',#21400,#17343,#17344);
#14943=AXIS2_PLACEMENT_3D('',#21403,#17346,#17347);
#14944=AXIS2_PLACEMENT_3D('',#21404,#17348,#17349);
#14945=AXIS2_PLACEMENT_3D('',#21406,#17350,#17351);
#14946=AXIS2_PLACEMENT_3D('',#21409,#17353,#17354);
#14947=AXIS2_PLACEMENT_3D('',#21410,#17355,#17356);
#14948=AXIS2_PLACEMENT_3D('',#21412,#17357,#17358);
#14949=AXIS2_PLACEMENT_3D('',#21415,#17360,#17361);
#14950=AXIS2_PLACEMENT_3D('',#21416,#17362,#17363);
#14951=AXIS2_PLACEMENT_3D('',#21418,#17364,#17365);
#14952=AXIS2_PLACEMENT_3D('',#21421,#17367,#17368);
#14953=AXIS2_PLACEMENT_3D('',#21422,#17369,#17370);
#14954=AXIS2_PLACEMENT_3D('',#21424,#17371,#17372);
#14955=AXIS2_PLACEMENT_3D('',#21427,#17374,#17375);
#14956=AXIS2_PLACEMENT_3D('',#21428,#17376,#17377);
#14957=AXIS2_PLACEMENT_3D('',#21437,#17382,#17383);
#14958=AXIS2_PLACEMENT_3D('',#21443,#17387,#17388);
#14959=AXIS2_PLACEMENT_3D('',#21449,#17392,#17393);
#14960=AXIS2_PLACEMENT_3D('',#21452,#17396,#17397);
#14961=AXIS2_PLACEMENT_3D('',#21453,#17398,#17399);
#14962=AXIS2_PLACEMENT_3D('',#21454,#17400,#17401);
#14963=AXIS2_PLACEMENT_3D('',#21455,#17402,#17403);
#14964=AXIS2_PLACEMENT_3D('',#21457,#17404,#17405);
#14965=AXIS2_PLACEMENT_3D('',#21460,#17407,#17408);
#14966=AXIS2_PLACEMENT_3D('',#21461,#17409,#17410);
#14967=AXIS2_PLACEMENT_3D('',#21462,#17411,#17412);
#14968=AXIS2_PLACEMENT_3D('',#21464,#17413,#17414);
#14969=AXIS2_PLACEMENT_3D('',#21467,#17416,#17417);
#14970=AXIS2_PLACEMENT_3D('',#21468,#17418,#17419);
#14971=AXIS2_PLACEMENT_3D('',#21469,#17420,#17421);
#14972=AXIS2_PLACEMENT_3D('',#21471,#17422,#17423);
#14973=AXIS2_PLACEMENT_3D('',#21474,#17425,#17426);
#14974=AXIS2_PLACEMENT_3D('',#21475,#17427,#17428);
#14975=AXIS2_PLACEMENT_3D('',#21476,#17429,#17430);
#14976=AXIS2_PLACEMENT_3D('',#21478,#17431,#17432);
#14977=AXIS2_PLACEMENT_3D('',#21481,#17434,#17435);
#14978=AXIS2_PLACEMENT_3D('',#21482,#17436,#17437);
#14979=AXIS2_PLACEMENT_3D('',#21483,#17438,#17439);
#14980=AXIS2_PLACEMENT_3D('',#21492,#17444,#17445);
#14981=AXIS2_PLACEMENT_3D('',#21498,#17449,#17450);
#14982=AXIS2_PLACEMENT_3D('',#21504,#17454,#17455);
#14983=AXIS2_PLACEMENT_3D('',#21510,#17459,#17460);
#14984=AXIS2_PLACEMENT_3D('',#21516,#17464,#17465);
#14985=AXIS2_PLACEMENT_3D('',#21522,#17469,#17470);
#14986=AXIS2_PLACEMENT_3D('',#21528,#17474,#17475);
#14987=AXIS2_PLACEMENT_3D('',#21534,#17479,#17480);
#14988=AXIS2_PLACEMENT_3D('',#21540,#17484,#17485);
#14989=AXIS2_PLACEMENT_3D('',#21546,#17489,#17490);
#14990=AXIS2_PLACEMENT_3D('',#21552,#17494,#17495);
#14991=AXIS2_PLACEMENT_3D('',#21558,#17499,#17500);
#14992=AXIS2_PLACEMENT_3D('',#21564,#17504,#17505);
#14993=AXIS2_PLACEMENT_3D('',#21570,#17509,#17510);
#14994=AXIS2_PLACEMENT_3D('',#21576,#17514,#17515);
#14995=AXIS2_PLACEMENT_3D('',#21582,#17519,#17520);
#14996=AXIS2_PLACEMENT_3D('',#21588,#17524,#17525);
#14997=AXIS2_PLACEMENT_3D('',#21594,#17529,#17530);
#14998=AXIS2_PLACEMENT_3D('',#21600,#17534,#17535);
#14999=AXIS2_PLACEMENT_3D('',#21606,#17539,#17540);
#15000=AXIS2_PLACEMENT_3D('',#21612,#17544,#17545);
#15001=AXIS2_PLACEMENT_3D('',#21618,#17549,#17550);
#15002=AXIS2_PLACEMENT_3D('',#21624,#17554,#17555);
#15003=AXIS2_PLACEMENT_3D('',#21630,#17559,#17560);
#15004=AXIS2_PLACEMENT_3D('',#21636,#17564,#17565);
#15005=AXIS2_PLACEMENT_3D('',#21642,#17569,#17570);
#15006=AXIS2_PLACEMENT_3D('',#21648,#17574,#17575);
#15007=AXIS2_PLACEMENT_3D('',#21654,#17579,#17580);
#15008=AXIS2_PLACEMENT_3D('',#21660,#17584,#17585);
#15009=AXIS2_PLACEMENT_3D('',#21666,#17589,#17590);
#15010=AXIS2_PLACEMENT_3D('',#21672,#17594,#17595);
#15011=AXIS2_PLACEMENT_3D('',#21678,#17599,#17600);
#15012=AXIS2_PLACEMENT_3D('',#21684,#17604,#17605);
#15013=AXIS2_PLACEMENT_3D('',#21690,#17609,#17610);
#15014=AXIS2_PLACEMENT_3D('',#21696,#17614,#17615);
#15015=AXIS2_PLACEMENT_3D('',#21702,#17619,#17620);
#15016=AXIS2_PLACEMENT_3D('',#21708,#17624,#17625);
#15017=AXIS2_PLACEMENT_3D('',#21714,#17629,#17630);
#15018=AXIS2_PLACEMENT_3D('',#21720,#17634,#17635);
#15019=AXIS2_PLACEMENT_3D('',#21726,#17639,#17640);
#15020=AXIS2_PLACEMENT_3D('',#21732,#17644,#17645);
#15021=AXIS2_PLACEMENT_3D('',#21738,#17649,#17650);
#15022=AXIS2_PLACEMENT_3D('',#21744,#17654,#17655);
#15023=AXIS2_PLACEMENT_3D('',#21750,#17659,#17660);
#15024=AXIS2_PLACEMENT_3D('',#21756,#17664,#17665);
#15025=AXIS2_PLACEMENT_3D('',#21762,#17669,#17670);
#15026=AXIS2_PLACEMENT_3D('',#21768,#17674,#17675);
#15027=AXIS2_PLACEMENT_3D('',#21774,#17679,#17680);
#15028=AXIS2_PLACEMENT_3D('',#21780,#17684,#17685);
#15029=AXIS2_PLACEMENT_3D('',#21786,#17689,#17690);
#15030=AXIS2_PLACEMENT_3D('',#21792,#17694,#17695);
#15031=AXIS2_PLACEMENT_3D('',#21798,#17699,#17700);
#15032=AXIS2_PLACEMENT_3D('',#21804,#17704,#17705);
#15033=AXIS2_PLACEMENT_3D('',#21810,#17709,#17710);
#15034=AXIS2_PLACEMENT_3D('',#21816,#17714,#17715);
#15035=AXIS2_PLACEMENT_3D('',#21822,#17719,#17720);
#15036=AXIS2_PLACEMENT_3D('',#21828,#17724,#17725);
#15037=AXIS2_PLACEMENT_3D('',#21834,#17729,#17730);
#15038=AXIS2_PLACEMENT_3D('',#21840,#17734,#17735);
#15039=AXIS2_PLACEMENT_3D('',#21846,#17739,#17740);
#15040=AXIS2_PLACEMENT_3D('',#21852,#17744,#17745);
#15041=AXIS2_PLACEMENT_3D('',#21858,#17749,#17750);
#15042=AXIS2_PLACEMENT_3D('',#21864,#17754,#17755);
#15043=AXIS2_PLACEMENT_3D('',#21870,#17759,#17760);
#15044=AXIS2_PLACEMENT_3D('',#21876,#17764,#17765);
#15045=AXIS2_PLACEMENT_3D('',#21882,#17769,#17770);
#15046=AXIS2_PLACEMENT_3D('',#21888,#17774,#17775);
#15047=AXIS2_PLACEMENT_3D('',#21894,#17779,#17780);
#15048=AXIS2_PLACEMENT_3D('',#21900,#17784,#17785);
#15049=AXIS2_PLACEMENT_3D('',#21906,#17789,#17790);
#15050=AXIS2_PLACEMENT_3D('',#21912,#17794,#17795);
#15051=AXIS2_PLACEMENT_3D('',#21918,#17799,#17800);
#15052=AXIS2_PLACEMENT_3D('',#21924,#17804,#17805);
#15053=AXIS2_PLACEMENT_3D('',#21930,#17809,#17810);
#15054=AXIS2_PLACEMENT_3D('',#21936,#17814,#17815);
#15055=AXIS2_PLACEMENT_3D('',#21942,#17819,#17820);
#15056=AXIS2_PLACEMENT_3D('',#21948,#17824,#17825);
#15057=AXIS2_PLACEMENT_3D('',#21954,#17829,#17830);
#15058=AXIS2_PLACEMENT_3D('',#21960,#17834,#17835);
#15059=AXIS2_PLACEMENT_3D('',#21966,#17839,#17840);
#15060=AXIS2_PLACEMENT_3D('',#21972,#17844,#17845);
#15061=AXIS2_PLACEMENT_3D('',#21978,#17849,#17850);
#15062=AXIS2_PLACEMENT_3D('',#21984,#17854,#17855);
#15063=AXIS2_PLACEMENT_3D('',#21990,#17859,#17860);
#15064=AXIS2_PLACEMENT_3D('',#21996,#17864,#17865);
#15065=AXIS2_PLACEMENT_3D('',#22002,#17869,#17870);
#15066=AXIS2_PLACEMENT_3D('',#22008,#17874,#17875);
#15067=AXIS2_PLACEMENT_3D('',#22014,#17879,#17880);
#15068=AXIS2_PLACEMENT_3D('',#22020,#17884,#17885);
#15069=AXIS2_PLACEMENT_3D('',#22026,#17889,#17890);
#15070=AXIS2_PLACEMENT_3D('',#22032,#17894,#17895);
#15071=AXIS2_PLACEMENT_3D('',#22038,#17899,#17900);
#15072=AXIS2_PLACEMENT_3D('',#22044,#17904,#17905);
#15073=AXIS2_PLACEMENT_3D('',#22050,#17909,#17910);
#15074=AXIS2_PLACEMENT_3D('',#22056,#17914,#17915);
#15075=AXIS2_PLACEMENT_3D('',#22062,#17919,#17920);
#15076=AXIS2_PLACEMENT_3D('',#22068,#17924,#17925);
#15077=AXIS2_PLACEMENT_3D('',#22074,#17929,#17930);
#15078=AXIS2_PLACEMENT_3D('',#22080,#17934,#17935);
#15079=AXIS2_PLACEMENT_3D('',#22086,#17939,#17940);
#15080=AXIS2_PLACEMENT_3D('',#22092,#17944,#17945);
#15081=AXIS2_PLACEMENT_3D('',#22098,#17949,#17950);
#15082=AXIS2_PLACEMENT_3D('',#22104,#17954,#17955);
#15083=AXIS2_PLACEMENT_3D('',#22110,#17959,#17960);
#15084=AXIS2_PLACEMENT_3D('',#22116,#17964,#17965);
#15085=AXIS2_PLACEMENT_3D('',#22122,#17969,#17970);
#15086=AXIS2_PLACEMENT_3D('',#22128,#17974,#17975);
#15087=AXIS2_PLACEMENT_3D('',#22134,#17979,#17980);
#15088=AXIS2_PLACEMENT_3D('',#22140,#17984,#17985);
#15089=AXIS2_PLACEMENT_3D('',#22146,#17989,#17990);
#15090=AXIS2_PLACEMENT_3D('',#22152,#17994,#17995);
#15091=AXIS2_PLACEMENT_3D('',#22158,#17999,#18000);
#15092=AXIS2_PLACEMENT_3D('',#22164,#18004,#18005);
#15093=AXIS2_PLACEMENT_3D('',#22170,#18009,#18010);
#15094=AXIS2_PLACEMENT_3D('',#22176,#18014,#18015);
#15095=AXIS2_PLACEMENT_3D('',#22182,#18019,#18020);
#15096=AXIS2_PLACEMENT_3D('',#22188,#18024,#18025);
#15097=AXIS2_PLACEMENT_3D('',#22194,#18029,#18030);
#15098=AXIS2_PLACEMENT_3D('',#22200,#18034,#18035);
#15099=AXIS2_PLACEMENT_3D('',#22206,#18039,#18040);
#15100=AXIS2_PLACEMENT_3D('',#22212,#18044,#18045);
#15101=AXIS2_PLACEMENT_3D('',#22218,#18049,#18050);
#15102=AXIS2_PLACEMENT_3D('',#22224,#18054,#18055);
#15103=AXIS2_PLACEMENT_3D('',#22230,#18059,#18060);
#15104=AXIS2_PLACEMENT_3D('',#22236,#18064,#18065);
#15105=AXIS2_PLACEMENT_3D('',#22242,#18069,#18070);
#15106=AXIS2_PLACEMENT_3D('',#22248,#18074,#18075);
#15107=AXIS2_PLACEMENT_3D('',#22251,#18078,#18079);
#15108=AXIS2_PLACEMENT_3D('',#22252,#18080,#18081);
#15109=AXIS2_PLACEMENT_3D('',#22253,#18082,#18083);
#15110=AXIS2_PLACEMENT_3D('',#22254,#18084,#18085);
#15111=AXIS2_PLACEMENT_3D('',#22255,#18086,#18087);
#15112=AXIS2_PLACEMENT_3D('',#22259,#18089,#18090);
#15113=AXIS2_PLACEMENT_3D('',#22260,#18091,#18092);
#15114=AXIS2_PLACEMENT_3D('',#22264,#18094,#18095);
#15115=AXIS2_PLACEMENT_3D('',#22267,#18097,#18098);
#15116=AXIS2_PLACEMENT_3D('',#22269,#18099,#18100);
#15117=AXIS2_PLACEMENT_3D('',#22271,#18102,#18103);
#15118=AXIS2_PLACEMENT_3D('',#22275,#18105,#18106);
#15119=AXIS2_PLACEMENT_3D('',#22276,#18107,#18108);
#15120=AXIS2_PLACEMENT_3D('',#22280,#18110,#18111);
#15121=AXIS2_PLACEMENT_3D('',#22283,#18113,#18114);
#15122=AXIS2_PLACEMENT_3D('',#22285,#18115,#18116);
#15123=AXIS2_PLACEMENT_3D('',#22287,#18118,#18119);
#15124=AXIS2_PLACEMENT_3D('',#22291,#18121,#18122);
#15125=AXIS2_PLACEMENT_3D('',#22292,#18123,#18124);
#15126=AXIS2_PLACEMENT_3D('',#22296,#18126,#18127);
#15127=AXIS2_PLACEMENT_3D('',#22299,#18129,#18130);
#15128=AXIS2_PLACEMENT_3D('',#22301,#18131,#18132);
#15129=AXIS2_PLACEMENT_3D('',#22303,#18134,#18135);
#15130=AXIS2_PLACEMENT_3D('',#22307,#18137,#18138);
#15131=AXIS2_PLACEMENT_3D('',#22308,#18139,#18140);
#15132=AXIS2_PLACEMENT_3D('',#22312,#18142,#18143);
#15133=AXIS2_PLACEMENT_3D('',#22315,#18145,#18146);
#15134=AXIS2_PLACEMENT_3D('',#22317,#18147,#18148);
#15135=AXIS2_PLACEMENT_3D('',#22319,#18150,#18151);
#15136=AXIS2_PLACEMENT_3D('',#22330,#18158,#18159);
#15137=AXIS2_PLACEMENT_3D('',#22341,#18166,#18167);
#15138=AXIS2_PLACEMENT_3D('',#22360,#18178,#18179);
#15139=AXIS2_PLACEMENT_3D('',#22364,#18182,#18183);
#15140=AXIS2_PLACEMENT_3D('',#22368,#18186,#18187);
#15141=AXIS2_PLACEMENT_3D('',#22372,#18190,#18191);
#15142=AXIS2_PLACEMENT_3D('',#22376,#18194,#18195);
#15143=AXIS2_PLACEMENT_3D('',#22378,#18197,#18198);
#15144=AXIS2_PLACEMENT_3D('',#22382,#18201,#18202);
#15145=AXIS2_PLACEMENT_3D('',#22386,#18205,#18206);
#15146=AXIS2_PLACEMENT_3D('',#22390,#18209,#18210);
#15147=AXIS2_PLACEMENT_3D('',#22394,#18213,#18214);
#15148=AXIS2_PLACEMENT_3D('',#22396,#18216,#18217);
#15149=AXIS2_PLACEMENT_3D('',#22397,#18218,#18219);
#15150=AXIS2_PLACEMENT_3D('',#22398,#18220,#18221);
#15151=AXIS2_PLACEMENT_3D('',#22407,#18226,#18227);
#15152=AXIS2_PLACEMENT_3D('',#22413,#18231,#18232);
#15153=AXIS2_PLACEMENT_3D('',#22419,#18236,#18237);
#15154=AXIS2_PLACEMENT_3D('',#22425,#18241,#18242);
#15155=AXIS2_PLACEMENT_3D('',#22431,#18246,#18247);
#15156=AXIS2_PLACEMENT_3D('',#22437,#18251,#18252);
#15157=AXIS2_PLACEMENT_3D('',#22443,#18256,#18257);
#15158=AXIS2_PLACEMENT_3D('',#22446,#18260,#18261);
#15159=AXIS2_PLACEMENT_3D('',#22447,#18262,#18263);
#15160=AXIS2_PLACEMENT_3D('',#22448,#18264,#18265);
#15161=AXIS2_PLACEMENT_3D('',#22449,#18266,#18267);
#15162=AXIS2_PLACEMENT_3D('',#22458,#18272,#18273);
#15163=AXIS2_PLACEMENT_3D('',#22464,#18277,#18278);
#15164=AXIS2_PLACEMENT_3D('',#22470,#18282,#18283);
#15165=AXIS2_PLACEMENT_3D('',#22476,#18287,#18288);
#15166=AXIS2_PLACEMENT_3D('',#22482,#18292,#18293);
#15167=AXIS2_PLACEMENT_3D('',#22488,#18297,#18298);
#15168=AXIS2_PLACEMENT_3D('',#22494,#18302,#18303);
#15169=AXIS2_PLACEMENT_3D('',#22497,#18306,#18307);
#15170=AXIS2_PLACEMENT_3D('',#22498,#18308,#18309);
#15171=AXIS2_PLACEMENT_3D('',#22499,#18310,#18311);
#15172=AXIS2_PLACEMENT_3D('',#22500,#18312,#18313);
#15173=AXIS2_PLACEMENT_3D('',#22501,#18314,#18315);
#15174=AXIS2_PLACEMENT_3D('',#22502,#18316,#18317);
#15175=AXIS2_PLACEMENT_3D('',#22503,#18318,#18319);
#15176=AXIS2_PLACEMENT_3D('',#22512,#18324,#18325);
#15177=AXIS2_PLACEMENT_3D('',#22518,#18329,#18330);
#15178=AXIS2_PLACEMENT_3D('',#22524,#18334,#18335);
#15179=AXIS2_PLACEMENT_3D('',#22530,#18339,#18340);
#15180=AXIS2_PLACEMENT_3D('',#22536,#18344,#18345);
#15181=AXIS2_PLACEMENT_3D('',#22539,#18348,#18349);
#15182=AXIS2_PLACEMENT_3D('',#22540,#18350,#18351);
#15183=AXIS2_PLACEMENT_3D('',#22541,#18352,#18353);
#15184=AXIS2_PLACEMENT_3D('',#22543,#18354,#18355);
#15185=AXIS2_PLACEMENT_3D('',#22544,#18356,#18357);
#15186=AXIS2_PLACEMENT_3D('',#22546,#18358,#18359);
#15187=AXIS2_PLACEMENT_3D('',#22547,#18360,#18361);
#15188=AXIS2_PLACEMENT_3D('',#22549,#18362,#18363);
#15189=AXIS2_PLACEMENT_3D('',#22551,#18365,#18366);
#15190=AXIS2_PLACEMENT_3D('',#22553,#18367,#18368);
#15191=AXIS2_PLACEMENT_3D('',#22555,#18370,#18371);
#15192=AXIS2_PLACEMENT_3D('',#22557,#18372,#18373);
#15193=AXIS2_PLACEMENT_3D('',#22559,#18375,#18376);
#15194=AXIS2_PLACEMENT_3D('',#22561,#18377,#18378);
#15195=AXIS2_PLACEMENT_3D('',#22562,#18379,#18380);
#15196=AXIS2_PLACEMENT_3D('',#22564,#18381,#18382);
#15197=AXIS2_PLACEMENT_3D('',#22566,#18384,#18385);
#15198=AXIS2_PLACEMENT_3D('',#22568,#18387,#18388);
#15199=AXIS2_PLACEMENT_3D('',#22569,#18389,#18390);
#15200=AXIS2_PLACEMENT_3D('',#22570,#18391,#18392);
#15201=AXIS2_PLACEMENT_3D('',#22579,#18397,#18398);
#15202=AXIS2_PLACEMENT_3D('',#22581,#18399,#18400);
#15203=AXIS2_PLACEMENT_3D('',#22585,#18403,#18404);
#15204=AXIS2_PLACEMENT_3D('',#22591,#18408,#18409);
#15205=AXIS2_PLACEMENT_3D('',#22593,#18411,#18412);
#15206=AXIS2_PLACEMENT_3D('',#22594,#18413,#18414);
#15207=AXIS2_PLACEMENT_3D('',#22595,#18415,#18416);
#15208=AXIS2_PLACEMENT_3D('',#22597,#18417,#18418);
#15209=AXIS2_PLACEMENT_3D('',#22600,#18420,#18421);
#15210=AXIS2_PLACEMENT_3D('',#22601,#18422,#18423);
#15211=AXIS2_PLACEMENT_3D('',#22602,#18424,#18425);
#15212=AXIS2_PLACEMENT_3D('',#22604,#18426,#18427);
#15213=AXIS2_PLACEMENT_3D('',#22607,#18429,#18430);
#15214=AXIS2_PLACEMENT_3D('',#22608,#18431,#18432);
#15215=AXIS2_PLACEMENT_3D('',#22609,#18433,#18434);
#15216=AXIS2_PLACEMENT_3D('',#22618,#18439,#18440);
#15217=AXIS2_PLACEMENT_3D('',#22620,#18441,#18442);
#15218=AXIS2_PLACEMENT_3D('',#22624,#18445,#18446);
#15219=AXIS2_PLACEMENT_3D('',#22630,#18450,#18451);
#15220=AXIS2_PLACEMENT_3D('',#22632,#18453,#18454);
#15221=AXIS2_PLACEMENT_3D('',#22633,#18455,#18456);
#15222=AXIS2_PLACEMENT_3D('',#22634,#18457,#18458);
#15223=AXIS2_PLACEMENT_3D('',#22636,#18459,#18460);
#15224=AXIS2_PLACEMENT_3D('',#22638,#18461,#18462);
#15225=AXIS2_PLACEMENT_3D('',#22639,#18463,#18464);
#15226=AXIS2_PLACEMENT_3D('',#22641,#18465,#18466);
#15227=AXIS2_PLACEMENT_3D('',#22643,#18467,#18468);
#15228=AXIS2_PLACEMENT_3D('',#22644,#18469,#18470);
#15229=AXIS2_PLACEMENT_3D('',#22646,#18472,#18473);
#15230=AXIS2_PLACEMENT_3D('',#22649,#18475,#18476);
#15231=AXIS2_PLACEMENT_3D('',#22650,#18477,#18478);
#15232=AXIS2_PLACEMENT_3D('',#22652,#18479,#18480);
#15233=AXIS2_PLACEMENT_3D('',#22654,#18482,#18483);
#15234=AXIS2_PLACEMENT_3D('',#22655,#18484,#18485);
#15235=AXIS2_PLACEMENT_3D('',#22656,#18486,#18487);
#15236=AXIS2_PLACEMENT_3D('',#22657,#18488,#18489);
#15237=AXIS2_PLACEMENT_3D('',#22659,#18490,#18491);
#15238=AXIS2_PLACEMENT_3D('',#22662,#18493,#18494);
#15239=AXIS2_PLACEMENT_3D('',#22663,#18495,#18496);
#15240=AXIS2_PLACEMENT_3D('',#22665,#18497,#18498);
#15241=AXIS2_PLACEMENT_3D('',#22668,#18500,#18501);
#15242=AXIS2_PLACEMENT_3D('',#22669,#18502,#18503);
#15243=AXIS2_PLACEMENT_3D('',#22670,#18504,#18505);
#15244=AXIS2_PLACEMENT_3D('',#22671,#18506,#18507);
#15245=AXIS2_PLACEMENT_3D('',#22672,#18508,#18509);
#15246=AXIS2_PLACEMENT_3D('',#22674,#18510,#18511);
#15247=AXIS2_PLACEMENT_3D('',#22677,#18513,#18514);
#15248=AXIS2_PLACEMENT_3D('',#22678,#18515,#18516);
#15249=AXIS2_PLACEMENT_3D('',#22680,#18517,#18518);
#15250=AXIS2_PLACEMENT_3D('',#22683,#18520,#18521);
#15251=AXIS2_PLACEMENT_3D('',#22684,#18522,#18523);
#15252=AXIS2_PLACEMENT_3D('',#22685,#18524,#18525);
#15253=AXIS2_PLACEMENT_3D('',#22686,#18526,#18527);
#15254=AXIS2_PLACEMENT_3D('',#22687,#18528,#18529);
#15255=AXIS2_PLACEMENT_3D('',#22689,#18530,#18531);
#15256=AXIS2_PLACEMENT_3D('',#22692,#18533,#18534);
#15257=AXIS2_PLACEMENT_3D('',#22693,#18535,#18536);
#15258=AXIS2_PLACEMENT_3D('',#22695,#18537,#18538);
#15259=AXIS2_PLACEMENT_3D('',#22698,#18540,#18541);
#15260=AXIS2_PLACEMENT_3D('',#22699,#18542,#18543);
#15261=AXIS2_PLACEMENT_3D('',#22700,#18544,#18545);
#15262=AXIS2_PLACEMENT_3D('',#22701,#18546,#18547);
#15263=AXIS2_PLACEMENT_3D('',#22702,#18548,#18549);
#15264=AXIS2_PLACEMENT_3D('',#22704,#18550,#18551);
#15265=AXIS2_PLACEMENT_3D('',#22707,#18553,#18554);
#15266=AXIS2_PLACEMENT_3D('',#22708,#18555,#18556);
#15267=AXIS2_PLACEMENT_3D('',#22710,#18557,#18558);
#15268=AXIS2_PLACEMENT_3D('',#22713,#18560,#18561);
#15269=AXIS2_PLACEMENT_3D('',#22714,#18562,#18563);
#15270=AXIS2_PLACEMENT_3D('',#22715,#18564,#18565);
#15271=AXIS2_PLACEMENT_3D('',#22716,#18566,#18567);
#15272=AXIS2_PLACEMENT_3D('',#22717,#18568,#18569);
#15273=AXIS2_PLACEMENT_3D('',#22719,#18570,#18571);
#15274=AXIS2_PLACEMENT_3D('',#22722,#18573,#18574);
#15275=AXIS2_PLACEMENT_3D('',#22723,#18575,#18576);
#15276=AXIS2_PLACEMENT_3D('',#22725,#18577,#18578);
#15277=AXIS2_PLACEMENT_3D('',#22728,#18580,#18581);
#15278=AXIS2_PLACEMENT_3D('',#22729,#18582,#18583);
#15279=AXIS2_PLACEMENT_3D('',#22730,#18584,#18585);
#15280=AXIS2_PLACEMENT_3D('',#22731,#18586,#18587);
#15281=AXIS2_PLACEMENT_3D('',#22732,#18588,#18589);
#15282=AXIS2_PLACEMENT_3D('',#22734,#18590,#18591);
#15283=AXIS2_PLACEMENT_3D('',#22737,#18593,#18594);
#15284=AXIS2_PLACEMENT_3D('',#22738,#18595,#18596);
#15285=AXIS2_PLACEMENT_3D('',#22740,#18597,#18598);
#15286=AXIS2_PLACEMENT_3D('',#22743,#18600,#18601);
#15287=AXIS2_PLACEMENT_3D('',#22744,#18602,#18603);
#15288=AXIS2_PLACEMENT_3D('',#22745,#18604,#18605);
#15289=AXIS2_PLACEMENT_3D('',#22746,#18606,#18607);
#15290=AXIS2_PLACEMENT_3D('',#22747,#18608,#18609);
#15291=AXIS2_PLACEMENT_3D('',#22749,#18610,#18611);
#15292=AXIS2_PLACEMENT_3D('',#22752,#18613,#18614);
#15293=AXIS2_PLACEMENT_3D('',#22753,#18615,#18616);
#15294=AXIS2_PLACEMENT_3D('',#22762,#18621,#18622);
#15295=AXIS2_PLACEMENT_3D('',#22768,#18626,#18627);
#15296=AXIS2_PLACEMENT_3D('',#22774,#18631,#18632);
#15297=AXIS2_PLACEMENT_3D('',#22776,#18633,#18634);
#15298=AXIS2_PLACEMENT_3D('',#22777,#18635,#18636);
#15299=AXIS2_PLACEMENT_3D('',#22778,#18637,#18638);
#15300=AXIS2_PLACEMENT_3D('',#22779,#18639,#18640);
#15301=AXIS2_PLACEMENT_3D('',#22780,#18641,#18642);
#15302=AXIS2_PLACEMENT_3D('',#22785,#18644,#18645);
#15303=AXIS2_PLACEMENT_3D('',#22788,#18647,#18648);
#15304=AXIS2_PLACEMENT_3D('',#22789,#18649,#18650);
#15305=AXIS2_PLACEMENT_3D('',#22795,#18654,#18655);
#15306=AXIS2_PLACEMENT_3D('',#22798,#18657,#18658);
#15307=AXIS2_PLACEMENT_3D('',#22799,#18659,#18660);
#15308=AXIS2_PLACEMENT_3D('',#22803,#18663,#18664);
#15309=AXIS2_PLACEMENT_3D('',#22804,#18665,#18666);
#15310=AXIS2_PLACEMENT_3D('',#22805,#18667,#18668);
#15311=AXIS2_PLACEMENT_3D('',#22808,#18670,#18671);
#15312=AXIS2_PLACEMENT_3D('',#22809,#18672,#18673);
#15313=AXIS2_PLACEMENT_3D('',#22810,#18674,#18675);
#15314=AXIS2_PLACEMENT_3D('',#22811,#18676,#18677);
#15315=AXIS2_PLACEMENT_3D('',#22813,#18678,#18679);
#15316=AXIS2_PLACEMENT_3D('',#22816,#18681,#18682);
#15317=AXIS2_PLACEMENT_3D('',#22817,#18683,#18684);
#15318=AXIS2_PLACEMENT_3D('',#22819,#18685,#18686);
#15319=AXIS2_PLACEMENT_3D('',#22822,#18688,#18689);
#15320=AXIS2_PLACEMENT_3D('',#22823,#18690,#18691);
#15321=AXIS2_PLACEMENT_3D('',#22824,#18692,#18693);
#15322=AXIS2_PLACEMENT_3D('',#22825,#18694,#18695);
#15323=AXIS2_PLACEMENT_3D('',#22826,#18696,#18697);
#15324=AXIS2_PLACEMENT_3D('',#22835,#18702,#18703);
#15325=AXIS2_PLACEMENT_3D('',#22841,#18707,#18708);
#15326=AXIS2_PLACEMENT_3D('',#22847,#18712,#18713);
#15327=AXIS2_PLACEMENT_3D('',#22850,#18714,#18715);
#15328=AXIS2_PLACEMENT_3D('',#22996,#18717,#18718);
#15329=AXIS2_PLACEMENT_3D('',#23142,#18720,#18721);
#15330=AXIS2_PLACEMENT_3D('',#23288,#18723,#18724);
#15331=AXIS2_PLACEMENT_3D('',#23434,#18726,#18727);
#15332=AXIS2_PLACEMENT_3D('',#23580,#18729,#18730);
#15333=AXIS2_PLACEMENT_3D('',#23726,#18732,#18733);
#15334=AXIS2_PLACEMENT_3D('',#23872,#18735,#18736);
#15335=AXIS2_PLACEMENT_3D('',#24018,#18738,#18739);
#15336=AXIS2_PLACEMENT_3D('',#24164,#18741,#18742);
#15337=AXIS2_PLACEMENT_3D('',#24310,#18744,#18745);
#15338=AXIS2_PLACEMENT_3D('',#24456,#18747,#18748);
#15339=AXIS2_PLACEMENT_3D('',#24602,#18750,#18751);
#15340=AXIS2_PLACEMENT_3D('',#24748,#18753,#18754);
#15341=AXIS2_PLACEMENT_3D('',#24894,#18756,#18757);
#15342=AXIS2_PLACEMENT_3D('',#25040,#18759,#18760);
#15343=AXIS2_PLACEMENT_3D('',#25186,#18762,#18763);
#15344=AXIS2_PLACEMENT_3D('',#25332,#18765,#18766);
#15345=AXIS2_PLACEMENT_3D('',#25478,#18768,#18769);
#15346=AXIS2_PLACEMENT_3D('',#25624,#18771,#18772);
#15347=AXIS2_PLACEMENT_3D('',#25768,#18774,#18775);
#15348=AXIS2_PLACEMENT_3D('',#25769,#18776,#18777);
#15349=AXIS2_PLACEMENT_3D('',#25770,#18778,#18779);
#15350=AXIS2_PLACEMENT_3D('',#25771,#18780,#18781);
#15351=AXIS2_PLACEMENT_3D('',#25773,#18782,#18783);
#15352=AXIS2_PLACEMENT_3D('',#25776,#18785,#18786);
#15353=AXIS2_PLACEMENT_3D('',#25777,#18787,#18788);
#15354=AXIS2_PLACEMENT_3D('',#25992,#18791,#18792);
#15355=AXIS2_PLACEMENT_3D('',#26208,#18796,#18797);
#15356=AXIS2_PLACEMENT_3D('',#26210,#18798,#18799);
#15357=AXIS2_PLACEMENT_3D('',#26424,#18802,#18803);
#15358=AXIS2_PLACEMENT_3D('',#26640,#18807,#18808);
#15359=AXIS2_PLACEMENT_3D('',#26642,#18809,#18810);
#15360=AXIS2_PLACEMENT_3D('',#26856,#18813,#18814);
#15361=AXIS2_PLACEMENT_3D('',#27072,#18818,#18819);
#15362=AXIS2_PLACEMENT_3D('',#27074,#18820,#18821);
#15363=AXIS2_PLACEMENT_3D('',#27288,#18824,#18825);
#15364=AXIS2_PLACEMENT_3D('',#27504,#18829,#18830);
#15365=AXIS2_PLACEMENT_3D('',#27506,#18831,#18832);
#15366=AXIS2_PLACEMENT_3D('',#27720,#18835,#18836);
#15367=AXIS2_PLACEMENT_3D('',#27936,#18840,#18841);
#15368=AXIS2_PLACEMENT_3D('',#27938,#18842,#18843);
#15369=AXIS2_PLACEMENT_3D('',#28152,#18846,#18847);
#15370=AXIS2_PLACEMENT_3D('',#28368,#18851,#18852);
#15371=AXIS2_PLACEMENT_3D('',#28370,#18853,#18854);
#15372=AXIS2_PLACEMENT_3D('',#28584,#18857,#18858);
#15373=AXIS2_PLACEMENT_3D('',#28800,#18862,#18863);
#15374=AXIS2_PLACEMENT_3D('',#28802,#18864,#18865);
#15375=AXIS2_PLACEMENT_3D('',#29016,#18868,#18869);
#15376=AXIS2_PLACEMENT_3D('',#29232,#18873,#18874);
#15377=AXIS2_PLACEMENT_3D('',#29234,#18875,#18876);
#15378=AXIS2_PLACEMENT_3D('',#29448,#18879,#18880);
#15379=AXIS2_PLACEMENT_3D('',#29664,#18884,#18885);
#15380=AXIS2_PLACEMENT_3D('',#29666,#18886,#18887);
#15381=AXIS2_PLACEMENT_3D('',#29880,#18890,#18891);
#15382=AXIS2_PLACEMENT_3D('',#30096,#18895,#18896);
#15383=AXIS2_PLACEMENT_3D('',#30098,#18897,#18898);
#15384=AXIS2_PLACEMENT_3D('',#30312,#18901,#18902);
#15385=AXIS2_PLACEMENT_3D('',#30528,#18906,#18907);
#15386=AXIS2_PLACEMENT_3D('',#30530,#18908,#18909);
#15387=AXIS2_PLACEMENT_3D('',#30744,#18912,#18913);
#15388=AXIS2_PLACEMENT_3D('',#30960,#18917,#18918);
#15389=AXIS2_PLACEMENT_3D('',#30962,#18919,#18920);
#15390=AXIS2_PLACEMENT_3D('',#31176,#18923,#18924);
#15391=AXIS2_PLACEMENT_3D('',#31392,#18928,#18929);
#15392=AXIS2_PLACEMENT_3D('',#31394,#18930,#18931);
#15393=AXIS2_PLACEMENT_3D('',#31608,#18934,#18935);
#15394=AXIS2_PLACEMENT_3D('',#31824,#18939,#18940);
#15395=AXIS2_PLACEMENT_3D('',#31826,#18941,#18942);
#15396=AXIS2_PLACEMENT_3D('',#32040,#18945,#18946);
#15397=AXIS2_PLACEMENT_3D('',#32256,#18950,#18951);
#15398=AXIS2_PLACEMENT_3D('',#32258,#18952,#18953);
#15399=AXIS2_PLACEMENT_3D('',#32472,#18956,#18957);
#15400=AXIS2_PLACEMENT_3D('',#32688,#18961,#18962);
#15401=AXIS2_PLACEMENT_3D('',#32690,#18963,#18964);
#15402=AXIS2_PLACEMENT_3D('',#32904,#18967,#18968);
#15403=AXIS2_PLACEMENT_3D('',#33120,#18972,#18973);
#15404=AXIS2_PLACEMENT_3D('',#33122,#18974,#18975);
#15405=AXIS2_PLACEMENT_3D('',#33336,#18978,#18979);
#15406=AXIS2_PLACEMENT_3D('',#33552,#18983,#18984);
#15407=AXIS2_PLACEMENT_3D('',#33554,#18985,#18986);
#15408=AXIS2_PLACEMENT_3D('',#33768,#18989,#18990);
#15409=AXIS2_PLACEMENT_3D('',#33984,#18994,#18995);
#15410=AXIS2_PLACEMENT_3D('',#33986,#18996,#18997);
#15411=AXIS2_PLACEMENT_3D('',#34200,#19000,#19001);
#15412=AXIS2_PLACEMENT_3D('',#34416,#19005,#19006);
#15413=AXIS2_PLACEMENT_3D('',#34417,#19007,#19008);
#15414=AXIS2_PLACEMENT_3D('',#34418,#19009,#19010);
#15415=AXIS2_PLACEMENT_3D('',#34419,#19011,#19012);
#15416=AXIS2_PLACEMENT_3D('',#34420,#19013,#19014);
#15417=AXIS2_PLACEMENT_3D('',#34422,#19015,#19016);
#15418=AXIS2_PLACEMENT_3D('',#34423,#19017,#19018);
#15419=AXIS2_PLACEMENT_3D('',#34425,#19019,#19020);
#15420=AXIS2_PLACEMENT_3D('',#34427,#19022,#19023);
#15421=AXIS2_PLACEMENT_3D('',#34429,#19024,#19025);
#15422=AXIS2_PLACEMENT_3D('',#34431,#19027,#19028);
#15423=AXIS2_PLACEMENT_3D('',#34433,#19029,#19030);
#15424=AXIS2_PLACEMENT_3D('',#34435,#19032,#19033);
#15425=AXIS2_PLACEMENT_3D('',#34437,#19034,#19035);
#15426=AXIS2_PLACEMENT_3D('',#34438,#19036,#19037);
#15427=AXIS2_PLACEMENT_3D('',#34440,#19038,#19039);
#15428=AXIS2_PLACEMENT_3D('',#34442,#19041,#19042);
#15429=AXIS2_PLACEMENT_3D('',#34444,#19043,#19044);
#15430=AXIS2_PLACEMENT_3D('',#34446,#19046,#19047);
#15431=AXIS2_PLACEMENT_3D('',#34448,#19048,#19049);
#15432=AXIS2_PLACEMENT_3D('',#34450,#19051,#19052);
#15433=AXIS2_PLACEMENT_3D('',#34451,#19053,#19054);
#15434=AXIS2_PLACEMENT_3D('',#34460,#19059,#19060);
#15435=AXIS2_PLACEMENT_3D('',#34466,#19064,#19065);
#15436=AXIS2_PLACEMENT_3D('',#34472,#19069,#19070);
#15437=AXIS2_PLACEMENT_3D('',#34478,#19074,#19075);
#15438=AXIS2_PLACEMENT_3D('',#34484,#19079,#19080);
#15439=AXIS2_PLACEMENT_3D('',#34487,#19083,#19084);
#15440=AXIS2_PLACEMENT_3D('',#34488,#19085,#19086);
#15441=AXIS2_PLACEMENT_3D('',#34489,#19087,#19088);
#15442=AXIS2_PLACEMENT_3D('',#34490,#19089,#19090);
#15443=AXIS2_PLACEMENT_3D('',#34491,#19091,#19092);
#15444=AXIS2_PLACEMENT_3D('',#34492,#19093,#19094);
#15445=AXIS2_PLACEMENT_3D('',#34493,#19095,#19096);
#15446=AXIS2_PLACEMENT_3D('',#34494,#19097,#19098);
#15447=AXIS2_PLACEMENT_3D('',#34495,#19099,#19100);
#15448=AXIS2_PLACEMENT_3D('',#34496,#19101,#19102);
#15449=AXIS2_PLACEMENT_3D('',#34497,#19103,#19104);
#15450=AXIS2_PLACEMENT_3D('',#34498,#19105,#19106);
#15451=AXIS2_PLACEMENT_3D('',#34499,#19107,#19108);
#15452=AXIS2_PLACEMENT_3D('',#34500,#19109,#19110);
#15453=AXIS2_PLACEMENT_3D('',#34501,#19111,#19112);
#15454=AXIS2_PLACEMENT_3D('',#34502,#19113,#19114);
#15455=AXIS2_PLACEMENT_3D('',#34503,#19115,#19116);
#15456=AXIS2_PLACEMENT_3D('',#34504,#19117,#19118);
#15457=AXIS2_PLACEMENT_3D('',#34505,#19119,#19120);
#15458=AXIS2_PLACEMENT_3D('',#34506,#19121,#19122);
#15459=AXIS2_PLACEMENT_3D('',#34507,#19123,#19124);
#15460=AXIS2_PLACEMENT_3D('',#34508,#19125,#19126);
#15461=AXIS2_PLACEMENT_3D('',#34509,#19127,#19128);
#15462=AXIS2_PLACEMENT_3D('',#34510,#19129,#19130);
#15463=AXIS2_PLACEMENT_3D('',#34511,#19131,#19132);
#15464=AXIS2_PLACEMENT_3D('',#34512,#19133,#19134);
#15465=AXIS2_PLACEMENT_3D('',#34513,#19135,#19136);
#15466=AXIS2_PLACEMENT_3D('',#34514,#19137,#19138);
#15467=AXIS2_PLACEMENT_3D('',#34515,#19139,#19140);
#15468=AXIS2_PLACEMENT_3D('',#34516,#19141,#19142);
#15469=AXIS2_PLACEMENT_3D('',#34517,#19143,#19144);
#15470=AXIS2_PLACEMENT_3D('',#34518,#19145,#19146);
#15471=AXIS2_PLACEMENT_3D('',#34519,#19147,#19148);
#15472=AXIS2_PLACEMENT_3D('',#34520,#19149,#19150);
#15473=AXIS2_PLACEMENT_3D('',#34521,#19151,#19152);
#15474=AXIS2_PLACEMENT_3D('',#34522,#19153,#19154);
#15475=AXIS2_PLACEMENT_3D('',#34523,#19155,#19156);
#15476=AXIS2_PLACEMENT_3D('',#34524,#19157,#19158);
#15477=AXIS2_PLACEMENT_3D('',#34525,#19159,#19160);
#15478=AXIS2_PLACEMENT_3D('',#34526,#19161,#19162);
#15479=AXIS2_PLACEMENT_3D('',#34527,#19163,#19164);
#15480=AXIS2_PLACEMENT_3D('',#34528,#19165,#19166);
#15481=AXIS2_PLACEMENT_3D('',#34529,#19167,#19168);
#15482=AXIS2_PLACEMENT_3D('',#34530,#19169,#19170);
#15483=AXIS2_PLACEMENT_3D('',#34531,#19171,#19172);
#15484=AXIS2_PLACEMENT_3D('',#34532,#19173,#19174);
#15485=AXIS2_PLACEMENT_3D('',#34533,#19175,#19176);
#15486=AXIS2_PLACEMENT_3D('',#34534,#19177,#19178);
#15487=AXIS2_PLACEMENT_3D('',#34535,#19179,#19180);
#15488=AXIS2_PLACEMENT_3D('',#34536,#19181,#19182);
#15489=AXIS2_PLACEMENT_3D('',#34537,#19183,#19184);
#15490=AXIS2_PLACEMENT_3D('',#34538,#19185,#19186);
#15491=AXIS2_PLACEMENT_3D('',#34539,#19187,#19188);
#15492=AXIS2_PLACEMENT_3D('',#34540,#19189,#19190);
#15493=AXIS2_PLACEMENT_3D('',#34541,#19191,#19192);
#15494=AXIS2_PLACEMENT_3D('',#34542,#19193,#19194);
#15495=AXIS2_PLACEMENT_3D('',#34543,#19195,#19196);
#15496=AXIS2_PLACEMENT_3D('',#34544,#19197,#19198);
#15497=AXIS2_PLACEMENT_3D('',#34545,#19199,#19200);
#15498=AXIS2_PLACEMENT_3D('',#34546,#19201,#19202);
#15499=AXIS2_PLACEMENT_3D('',#34547,#19203,#19204);
#15500=AXIS2_PLACEMENT_3D('',#34548,#19205,#19206);
#15501=AXIS2_PLACEMENT_3D('',#34549,#19207,#19208);
#15502=AXIS2_PLACEMENT_3D('',#34550,#19209,#19210);
#15503=AXIS2_PLACEMENT_3D('',#34551,#19211,#19212);
#15504=AXIS2_PLACEMENT_3D('',#34552,#19213,#19214);
#15505=AXIS2_PLACEMENT_3D('',#34553,#19215,#19216);
#15506=AXIS2_PLACEMENT_3D('',#34554,#19217,#19218);
#15507=AXIS2_PLACEMENT_3D('',#34555,#19219,#19220);
#15508=AXIS2_PLACEMENT_3D('',#34556,#19221,#19222);
#15509=AXIS2_PLACEMENT_3D('',#34557,#19223,#19224);
#15510=AXIS2_PLACEMENT_3D('',#34558,#19225,#19226);
#15511=AXIS2_PLACEMENT_3D('',#34559,#19227,#19228);
#15512=AXIS2_PLACEMENT_3D('',#34560,#19229,#19230);
#15513=AXIS2_PLACEMENT_3D('',#34561,#19231,#19232);
#15514=AXIS2_PLACEMENT_3D('',#34562,#19233,#19234);
#15515=AXIS2_PLACEMENT_3D('',#34563,#19235,#19236);
#15516=AXIS2_PLACEMENT_3D('',#34564,#19237,#19238);
#15517=AXIS2_PLACEMENT_3D('',#34565,#19239,#19240);
#15518=AXIS2_PLACEMENT_3D('',#34566,#19241,#19242);
#15519=AXIS2_PLACEMENT_3D('',#34567,#19243,#19244);
#15520=AXIS2_PLACEMENT_3D('',#34568,#19245,#19246);
#15521=AXIS2_PLACEMENT_3D('',#34569,#19247,#19248);
#15522=AXIS2_PLACEMENT_3D('',#34570,#19249,#19250);
#15523=AXIS2_PLACEMENT_3D('',#34571,#19251,#19252);
#15524=AXIS2_PLACEMENT_3D('',#34572,#19253,#19254);
#15525=AXIS2_PLACEMENT_3D('',#34589,#19263,#19264);
#15526=AXIS2_PLACEMENT_3D('',#34595,#19268,#19269);
#15527=AXIS2_PLACEMENT_3D('',#34599,#19272,#19273);
#15528=AXIS2_PLACEMENT_3D('',#34603,#19276,#19277);
#15529=AXIS2_PLACEMENT_3D('',#34607,#19280,#19281);
#15530=AXIS2_PLACEMENT_3D('',#34615,#19286,#19287);
#15531=AXIS2_PLACEMENT_3D('',#34617,#19289,#19290);
#15532=AXIS2_PLACEMENT_3D('',#34619,#19292,#19293);
#15533=AXIS2_PLACEMENT_3D('',#34621,#19295,#19296);
#15534=AXIS2_PLACEMENT_3D('',#34622,#19297,#19298);
#15535=AXIS2_PLACEMENT_3D('',#34623,#19299,#19300);
#15536=AXIS2_PLACEMENT_3D('',#34625,#19301,#19302);
#15537=AXIS2_PLACEMENT_3D('',#34628,#19304,#19305);
#15538=AXIS2_PLACEMENT_3D('',#34629,#19306,#19307);
#15539=AXIS2_PLACEMENT_3D('',#34631,#19308,#19309);
#15540=AXIS2_PLACEMENT_3D('',#34634,#19311,#19312);
#15541=AXIS2_PLACEMENT_3D('',#34635,#19313,#19314);
#15542=AXIS2_PLACEMENT_3D('',#34636,#19315,#19316);
#15543=AXIS2_PLACEMENT_3D('',#34637,#19317,#19318);
#15544=AXIS2_PLACEMENT_3D('',#34638,#19319,#19320);
#15545=AXIS2_PLACEMENT_3D('',#34640,#19321,#19322);
#15546=AXIS2_PLACEMENT_3D('',#34641,#19323,#19324);
#15547=AXIS2_PLACEMENT_3D('',#34643,#19325,#19326);
#15548=AXIS2_PLACEMENT_3D('',#34645,#19328,#19329);
#15549=AXIS2_PLACEMENT_3D('',#34647,#19330,#19331);
#15550=AXIS2_PLACEMENT_3D('',#34649,#19333,#19334);
#15551=AXIS2_PLACEMENT_3D('',#34651,#19335,#19336);
#15552=AXIS2_PLACEMENT_3D('',#34653,#19338,#19339);
#15553=AXIS2_PLACEMENT_3D('',#34655,#19340,#19341);
#15554=AXIS2_PLACEMENT_3D('',#34656,#19342,#19343);
#15555=AXIS2_PLACEMENT_3D('',#34658,#19344,#19345);
#15556=AXIS2_PLACEMENT_3D('',#34660,#19347,#19348);
#15557=AXIS2_PLACEMENT_3D('',#34662,#19349,#19350);
#15558=AXIS2_PLACEMENT_3D('',#34664,#19352,#19353);
#15559=AXIS2_PLACEMENT_3D('',#34666,#19354,#19355);
#15560=AXIS2_PLACEMENT_3D('',#34668,#19357,#19358);
#15561=AXIS2_PLACEMENT_3D('',#34669,#19359,#19360);
#15562=AXIS2_PLACEMENT_3D('',#34678,#19365,#19366);
#15563=AXIS2_PLACEMENT_3D('',#34684,#19370,#19371);
#15564=AXIS2_PLACEMENT_3D('',#34690,#19375,#19376);
#15565=AXIS2_PLACEMENT_3D('',#34696,#19380,#19381);
#15566=AXIS2_PLACEMENT_3D('',#34702,#19385,#19386);
#15567=AXIS2_PLACEMENT_3D('',#34705,#19389,#19390);
#15568=AXIS2_PLACEMENT_3D('',#34706,#19391,#19392);
#15569=AXIS2_PLACEMENT_3D('',#34707,#19393,#19394);
#15570=AXIS2_PLACEMENT_3D('',#34708,#19395,#19396);
#15571=AXIS2_PLACEMENT_3D('',#34709,#19397,#19398);
#15572=AXIS2_PLACEMENT_3D('',#34710,#19399,#19400);
#15573=AXIS2_PLACEMENT_3D('',#34711,#19401,#19402);
#15574=AXIS2_PLACEMENT_3D('',#34712,#19403,#19404);
#15575=AXIS2_PLACEMENT_3D('',#34713,#19405,#19406);
#15576=AXIS2_PLACEMENT_3D('',#34714,#19407,#19408);
#15577=AXIS2_PLACEMENT_3D('',#34715,#19409,#19410);
#15578=AXIS2_PLACEMENT_3D('',#34716,#19411,#19412);
#15579=AXIS2_PLACEMENT_3D('',#34717,#19413,#19414);
#15580=AXIS2_PLACEMENT_3D('',#34718,#19415,#19416);
#15581=AXIS2_PLACEMENT_3D('',#34719,#19417,#19418);
#15582=AXIS2_PLACEMENT_3D('',#34720,#19419,#19420);
#15583=AXIS2_PLACEMENT_3D('',#34721,#19421,#19422);
#15584=AXIS2_PLACEMENT_3D('',#34722,#19423,#19424);
#15585=AXIS2_PLACEMENT_3D('',#34723,#19425,#19426);
#15586=AXIS2_PLACEMENT_3D('',#34724,#19427,#19428);
#15587=AXIS2_PLACEMENT_3D('',#34725,#19429,#19430);
#15588=AXIS2_PLACEMENT_3D('',#34727,#19431,#19432);
#15589=AXIS2_PLACEMENT_3D('',#34730,#19434,#19435);
#15590=AXIS2_PLACEMENT_3D('',#34731,#19436,#19437);
#15591=AXIS2_PLACEMENT_3D('',#34733,#19438,#19439);
#15592=AXIS2_PLACEMENT_3D('',#34736,#19441,#19442);
#15593=AXIS2_PLACEMENT_3D('',#34737,#19443,#19444);
#15594=AXIS2_PLACEMENT_3D('',#34738,#19445,#19446);
#15595=AXIS2_PLACEMENT_3D('',#34739,#19447,#19448);
#15596=AXIS2_PLACEMENT_3D('',#34740,#19449,#19450);
#15597=AXIS2_PLACEMENT_3D('',#34741,#19451,#19452);
#15598=AXIS2_PLACEMENT_3D('',#34742,#19453,#19454);
#15599=AXIS2_PLACEMENT_3D('',#34743,#19455,#19456);
#15600=DIRECTION('axis',(0.,0.,1.));
#15601=DIRECTION('refdir',(1.,0.,0.));
#15602=DIRECTION('axis',(0.,0.,1.));
#15603=DIRECTION('refdir',(1.,0.,0.));
#15604=DIRECTION('axis',(0.,0.,1.));
#15605=DIRECTION('refdir',(1.,0.,0.));
#15606=DIRECTION('center_axis',(0.,0.,1.));
#15607=DIRECTION('ref_axis',(1.,0.,0.));
#15608=DIRECTION('center_axis',(0.,0.,1.));
#15609=DIRECTION('ref_axis',(1.,0.,0.));
#15610=DIRECTION('',(0.,0.,1.));
#15611=DIRECTION('center_axis',(0.,0.,-1.));
#15612=DIRECTION('ref_axis',(1.,0.,0.));
#15613=DIRECTION('center_axis',(0.,0.,1.));
#15614=DIRECTION('ref_axis',(1.,0.,0.));
#15615=DIRECTION('center_axis',(0.,0.,1.));
#15616=DIRECTION('ref_axis',(1.,0.,0.));
#15617=DIRECTION('',(0.,0.,1.));
#15618=DIRECTION('center_axis',(0.,0.,-1.));
#15619=DIRECTION('ref_axis',(1.,0.,0.));
#15620=DIRECTION('center_axis',(0.,0.,1.));
#15621=DIRECTION('ref_axis',(1.,0.,0.));
#15622=DIRECTION('center_axis',(0.,0.,1.));
#15623=DIRECTION('ref_axis',(1.,0.,0.));
#15624=DIRECTION('',(0.,0.,1.));
#15625=DIRECTION('center_axis',(0.,0.,-1.));
#15626=DIRECTION('ref_axis',(1.,0.,0.));
#15627=DIRECTION('center_axis',(0.,0.,1.));
#15628=DIRECTION('ref_axis',(1.,0.,0.));
#15629=DIRECTION('center_axis',(0.,0.,1.));
#15630=DIRECTION('ref_axis',(1.,0.,0.));
#15631=DIRECTION('',(0.,0.,1.));
#15632=DIRECTION('center_axis',(0.,0.,-1.));
#15633=DIRECTION('ref_axis',(1.,0.,0.));
#15634=DIRECTION('center_axis',(0.,1.,0.));
#15635=DIRECTION('ref_axis',(-1.,0.,0.));
#15636=DIRECTION('',(-1.,0.,0.));
#15637=DIRECTION('',(0.,0.,1.));
#15638=DIRECTION('',(-1.,0.,0.));
#15639=DIRECTION('',(0.,0.,1.));
#15640=DIRECTION('center_axis',(1.,0.,0.));
#15641=DIRECTION('ref_axis',(0.,1.,0.));
#15642=DIRECTION('',(0.,1.,0.));
#15643=DIRECTION('',(0.,1.,0.));
#15644=DIRECTION('',(0.,0.,1.));
#15645=DIRECTION('center_axis',(0.,-1.,0.));
#15646=DIRECTION('ref_axis',(1.,0.,0.));
#15647=DIRECTION('',(1.,0.,0.));
#15648=DIRECTION('',(1.,0.,0.));
#15649=DIRECTION('',(0.,0.,1.));
#15650=DIRECTION('center_axis',(-1.,0.,0.));
#15651=DIRECTION('ref_axis',(0.,-1.,0.));
#15652=DIRECTION('',(0.,-1.,0.));
#15653=DIRECTION('',(0.,-1.,0.));
#15654=DIRECTION('center_axis',(0.,0.,1.));
#15655=DIRECTION('ref_axis',(1.,0.,0.));
#15656=DIRECTION('center_axis',(0.,0.,1.));
#15657=DIRECTION('ref_axis',(1.,0.,0.));
#15658=DIRECTION('axis',(0.,0.,1.));
#15659=DIRECTION('refdir',(1.,0.,0.));
#15660=DIRECTION('center_axis',(0.,1.,0.));
#15661=DIRECTION('ref_axis',(-1.,0.,0.));
#15662=DIRECTION('',(-1.,0.,0.));
#15663=DIRECTION('',(0.,0.,1.));
#15664=DIRECTION('',(-1.,0.,0.));
#15665=DIRECTION('',(0.,0.,1.));
#15666=DIRECTION('center_axis',(1.,0.,0.));
#15667=DIRECTION('ref_axis',(0.,1.,0.));
#15668=DIRECTION('',(0.,1.,0.));
#15669=DIRECTION('',(0.,1.,0.));
#15670=DIRECTION('',(0.,0.,1.));
#15671=DIRECTION('center_axis',(0.,-1.,0.));
#15672=DIRECTION('ref_axis',(1.,0.,0.));
#15673=DIRECTION('',(1.,0.,0.));
#15674=DIRECTION('',(1.,0.,0.));
#15675=DIRECTION('',(0.,0.,1.));
#15676=DIRECTION('center_axis',(-1.,0.,0.));
#15677=DIRECTION('ref_axis',(0.,-1.,0.));
#15678=DIRECTION('',(0.,-1.,0.));
#15679=DIRECTION('',(0.,-1.,0.));
#15680=DIRECTION('center_axis',(0.,0.,1.));
#15681=DIRECTION('ref_axis',(1.,0.,0.));
#15682=DIRECTION('center_axis',(0.,0.,1.));
#15683=DIRECTION('ref_axis',(1.,0.,0.));
#15684=DIRECTION('axis',(0.,0.,1.));
#15685=DIRECTION('refdir',(1.,0.,0.));
#15686=DIRECTION('center_axis',(0.,1.,0.));
#15687=DIRECTION('ref_axis',(-1.,0.,0.));
#15688=DIRECTION('',(-1.,0.,0.));
#15689=DIRECTION('',(0.,0.,1.));
#15690=DIRECTION('',(-1.,0.,0.));
#15691=DIRECTION('',(0.,0.,1.));
#15692=DIRECTION('center_axis',(1.,0.,0.));
#15693=DIRECTION('ref_axis',(0.,1.,0.));
#15694=DIRECTION('',(0.,1.,0.));
#15695=DIRECTION('',(0.,1.,0.));
#15696=DIRECTION('',(0.,0.,1.));
#15697=DIRECTION('center_axis',(0.,-1.,0.));
#15698=DIRECTION('ref_axis',(1.,0.,0.));
#15699=DIRECTION('',(1.,0.,0.));
#15700=DIRECTION('',(1.,0.,0.));
#15701=DIRECTION('',(0.,0.,1.));
#15702=DIRECTION('center_axis',(-1.,0.,0.));
#15703=DIRECTION('ref_axis',(0.,-1.,0.));
#15704=DIRECTION('',(0.,-1.,0.));
#15705=DIRECTION('',(0.,-1.,0.));
#15706=DIRECTION('center_axis',(0.,0.,1.));
#15707=DIRECTION('ref_axis',(1.,0.,0.));
#15708=DIRECTION('center_axis',(0.,0.,1.));
#15709=DIRECTION('ref_axis',(1.,0.,0.));
#15710=DIRECTION('axis',(0.,0.,1.));
#15711=DIRECTION('refdir',(1.,0.,0.));
#15712=DIRECTION('center_axis',(0.,0.,1.));
#15713=DIRECTION('ref_axis',(1.,0.,0.));
#15714=DIRECTION('center_axis',(0.,0.,1.));
#15715=DIRECTION('ref_axis',(1.,0.,0.));
#15716=DIRECTION('',(0.,0.,1.));
#15717=DIRECTION('center_axis',(0.,0.,-1.));
#15718=DIRECTION('ref_axis',(1.,0.,0.));
#15719=DIRECTION('center_axis',(0.,0.,1.));
#15720=DIRECTION('ref_axis',(1.,0.,0.));
#15721=DIRECTION('center_axis',(0.,0.,1.));
#15722=DIRECTION('ref_axis',(1.,0.,0.));
#15723=DIRECTION('',(0.,0.,1.));
#15724=DIRECTION('center_axis',(0.,0.,-1.));
#15725=DIRECTION('ref_axis',(1.,0.,0.));
#15726=DIRECTION('center_axis',(0.,0.,1.));
#15727=DIRECTION('ref_axis',(1.,0.,0.));
#15728=DIRECTION('center_axis',(0.,0.,1.));
#15729=DIRECTION('ref_axis',(1.,0.,0.));
#15730=DIRECTION('',(0.,0.,1.));
#15731=DIRECTION('center_axis',(0.,0.,-1.));
#15732=DIRECTION('ref_axis',(1.,0.,0.));
#15733=DIRECTION('center_axis',(0.,0.,1.));
#15734=DIRECTION('ref_axis',(1.,0.,0.));
#15735=DIRECTION('center_axis',(0.,0.,1.));
#15736=DIRECTION('ref_axis',(1.,0.,0.));
#15737=DIRECTION('',(0.,0.,1.));
#15738=DIRECTION('center_axis',(0.,0.,-1.));
#15739=DIRECTION('ref_axis',(1.,0.,0.));
#15740=DIRECTION('center_axis',(0.,0.,1.));
#15741=DIRECTION('ref_axis',(1.,0.,0.));
#15742=DIRECTION('center_axis',(0.,0.,1.));
#15743=DIRECTION('ref_axis',(1.,0.,0.));
#15744=DIRECTION('',(0.,0.,1.));
#15745=DIRECTION('center_axis',(0.,0.,-1.));
#15746=DIRECTION('ref_axis',(1.,0.,0.));
#15747=DIRECTION('center_axis',(0.,0.,1.));
#15748=DIRECTION('ref_axis',(1.,0.,0.));
#15749=DIRECTION('center_axis',(0.,0.,1.));
#15750=DIRECTION('ref_axis',(1.,0.,0.));
#15751=DIRECTION('',(0.,0.,1.));
#15752=DIRECTION('center_axis',(0.,0.,-1.));
#15753=DIRECTION('ref_axis',(1.,0.,0.));
#15754=DIRECTION('center_axis',(0.,0.,1.));
#15755=DIRECTION('ref_axis',(1.,0.,0.));
#15756=DIRECTION('center_axis',(0.,0.,1.));
#15757=DIRECTION('ref_axis',(1.,0.,0.));
#15758=DIRECTION('',(0.,0.,1.));
#15759=DIRECTION('center_axis',(0.,0.,-1.));
#15760=DIRECTION('ref_axis',(1.,0.,0.));
#15761=DIRECTION('center_axis',(0.,0.,1.));
#15762=DIRECTION('ref_axis',(1.,0.,0.));
#15763=DIRECTION('center_axis',(0.,0.,1.));
#15764=DIRECTION('ref_axis',(1.,0.,0.));
#15765=DIRECTION('',(0.,0.,1.));
#15766=DIRECTION('center_axis',(0.,0.,-1.));
#15767=DIRECTION('ref_axis',(1.,0.,0.));
#15768=DIRECTION('center_axis',(0.,0.,1.));
#15769=DIRECTION('ref_axis',(1.,0.,0.));
#15770=DIRECTION('center_axis',(0.,0.,1.));
#15771=DIRECTION('ref_axis',(1.,0.,0.));
#15772=DIRECTION('',(0.,0.,1.));
#15773=DIRECTION('center_axis',(0.,0.,-1.));
#15774=DIRECTION('ref_axis',(1.,0.,0.));
#15775=DIRECTION('center_axis',(0.,0.,1.));
#15776=DIRECTION('ref_axis',(1.,0.,0.));
#15777=DIRECTION('center_axis',(0.,0.,1.));
#15778=DIRECTION('ref_axis',(1.,0.,0.));
#15779=DIRECTION('',(0.,0.,1.));
#15780=DIRECTION('center_axis',(0.,0.,-1.));
#15781=DIRECTION('ref_axis',(1.,0.,0.));
#15782=DIRECTION('center_axis',(0.,0.,1.));
#15783=DIRECTION('ref_axis',(1.,0.,0.));
#15784=DIRECTION('center_axis',(0.,0.,1.));
#15785=DIRECTION('ref_axis',(1.,0.,0.));
#15786=DIRECTION('',(0.,0.,1.));
#15787=DIRECTION('center_axis',(0.,0.,-1.));
#15788=DIRECTION('ref_axis',(1.,0.,0.));
#15789=DIRECTION('center_axis',(0.,0.,1.));
#15790=DIRECTION('ref_axis',(1.,0.,0.));
#15791=DIRECTION('center_axis',(0.,0.,1.));
#15792=DIRECTION('ref_axis',(1.,0.,0.));
#15793=DIRECTION('',(0.,0.,1.));
#15794=DIRECTION('center_axis',(0.,0.,-1.));
#15795=DIRECTION('ref_axis',(1.,0.,0.));
#15796=DIRECTION('center_axis',(0.,0.,1.));
#15797=DIRECTION('ref_axis',(1.,0.,0.));
#15798=DIRECTION('center_axis',(0.,0.,1.));
#15799=DIRECTION('ref_axis',(1.,0.,0.));
#15800=DIRECTION('',(0.,0.,1.));
#15801=DIRECTION('center_axis',(0.,0.,-1.));
#15802=DIRECTION('ref_axis',(1.,0.,0.));
#15803=DIRECTION('center_axis',(0.,0.,1.));
#15804=DIRECTION('ref_axis',(1.,0.,0.));
#15805=DIRECTION('center_axis',(0.,0.,1.));
#15806=DIRECTION('ref_axis',(1.,0.,0.));
#15807=DIRECTION('',(0.,0.,1.));
#15808=DIRECTION('center_axis',(0.,0.,-1.));
#15809=DIRECTION('ref_axis',(1.,0.,0.));
#15810=DIRECTION('center_axis',(0.,0.,1.));
#15811=DIRECTION('ref_axis',(1.,0.,0.));
#15812=DIRECTION('center_axis',(0.,0.,1.));
#15813=DIRECTION('ref_axis',(1.,0.,0.));
#15814=DIRECTION('',(0.,0.,1.));
#15815=DIRECTION('center_axis',(0.,0.,-1.));
#15816=DIRECTION('ref_axis',(1.,0.,0.));
#15817=DIRECTION('center_axis',(0.,0.,1.));
#15818=DIRECTION('ref_axis',(1.,0.,0.));
#15819=DIRECTION('center_axis',(0.,0.,1.));
#15820=DIRECTION('ref_axis',(1.,0.,0.));
#15821=DIRECTION('',(0.,0.,1.));
#15822=DIRECTION('center_axis',(0.,0.,-1.));
#15823=DIRECTION('ref_axis',(1.,0.,0.));
#15824=DIRECTION('center_axis',(0.,1.,0.));
#15825=DIRECTION('ref_axis',(-1.,0.,0.));
#15826=DIRECTION('',(-1.,0.,0.));
#15827=DIRECTION('',(0.,0.,1.));
#15828=DIRECTION('',(-1.,0.,0.));
#15829=DIRECTION('',(0.,0.,1.));
#15830=DIRECTION('center_axis',(1.,0.,0.));
#15831=DIRECTION('ref_axis',(0.,1.,0.));
#15832=DIRECTION('',(0.,1.,0.));
#15833=DIRECTION('',(0.,1.,0.));
#15834=DIRECTION('',(0.,0.,1.));
#15835=DIRECTION('center_axis',(0.,-1.,0.));
#15836=DIRECTION('ref_axis',(1.,0.,0.));
#15837=DIRECTION('',(1.,0.,0.));
#15838=DIRECTION('',(1.,0.,0.));
#15839=DIRECTION('',(0.,0.,1.));
#15840=DIRECTION('center_axis',(-1.,0.,0.));
#15841=DIRECTION('ref_axis',(0.,-1.,0.));
#15842=DIRECTION('',(0.,-1.,0.));
#15843=DIRECTION('',(0.,-1.,0.));
#15844=DIRECTION('center_axis',(0.,0.,1.));
#15845=DIRECTION('ref_axis',(1.,0.,0.));
#15846=DIRECTION('center_axis',(0.,0.,1.));
#15847=DIRECTION('ref_axis',(1.,0.,0.));
#15848=DIRECTION('axis',(0.,0.,1.));
#15849=DIRECTION('refdir',(1.,0.,0.));
#15850=DIRECTION('center_axis',(0.,0.,1.));
#15851=DIRECTION('ref_axis',(1.,0.,0.));
#15852=DIRECTION('center_axis',(0.,0.,1.));
#15853=DIRECTION('ref_axis',(1.,0.,0.));
#15854=DIRECTION('',(0.,0.,1.));
#15855=DIRECTION('center_axis',(0.,0.,-1.));
#15856=DIRECTION('ref_axis',(1.,0.,0.));
#15857=DIRECTION('center_axis',(0.,0.,1.));
#15858=DIRECTION('ref_axis',(1.,0.,0.));
#15859=DIRECTION('center_axis',(0.,0.,1.));
#15860=DIRECTION('ref_axis',(1.,0.,0.));
#15861=DIRECTION('center_axis',(0.,0.,1.));
#15862=DIRECTION('ref_axis',(1.,0.,0.));
#15863=DIRECTION('center_axis',(0.,0.,1.));
#15864=DIRECTION('ref_axis',(1.,0.,0.));
#15865=DIRECTION('',(0.,0.,1.));
#15866=DIRECTION('center_axis',(0.,0.,-1.));
#15867=DIRECTION('ref_axis',(1.,0.,0.));
#15868=DIRECTION('center_axis',(0.,0.,1.));
#15869=DIRECTION('ref_axis',(1.,0.,0.));
#15870=DIRECTION('center_axis',(0.,0.,1.));
#15871=DIRECTION('ref_axis',(1.,0.,0.));
#15872=DIRECTION('center_axis',(0.,0.,1.));
#15873=DIRECTION('ref_axis',(1.,0.,0.));
#15874=DIRECTION('center_axis',(0.,0.,1.));
#15875=DIRECTION('ref_axis',(1.,0.,0.));
#15876=DIRECTION('',(0.,0.,1.));
#15877=DIRECTION('center_axis',(0.,0.,1.));
#15878=DIRECTION('ref_axis',(1.,0.,0.));
#15879=DIRECTION('center_axis',(0.,0.,1.));
#15880=DIRECTION('ref_axis',(1.,0.,0.));
#15881=DIRECTION('',(0.,0.,1.));
#15882=DIRECTION('center_axis',(0.,1.,0.));
#15883=DIRECTION('ref_axis',(-1.,0.,0.));
#15884=DIRECTION('',(-1.,0.,0.));
#15885=DIRECTION('',(0.,0.,1.));
#15886=DIRECTION('',(-1.,0.,0.));
#15887=DIRECTION('',(0.,0.,1.));
#15888=DIRECTION('center_axis',(1.,0.,0.));
#15889=DIRECTION('ref_axis',(0.,1.,0.));
#15890=DIRECTION('',(0.,1.,0.));
#15891=DIRECTION('',(0.,1.,0.));
#15892=DIRECTION('',(0.,0.,1.));
#15893=DIRECTION('center_axis',(0.,-1.,0.));
#15894=DIRECTION('ref_axis',(1.,0.,0.));
#15895=DIRECTION('',(1.,0.,0.));
#15896=DIRECTION('',(1.,0.,0.));
#15897=DIRECTION('',(0.,0.,1.));
#15898=DIRECTION('center_axis',(-1.,0.,0.));
#15899=DIRECTION('ref_axis',(0.,-1.,0.));
#15900=DIRECTION('',(0.,-1.,0.));
#15901=DIRECTION('',(0.,-1.,0.));
#15902=DIRECTION('center_axis',(0.,0.,1.));
#15903=DIRECTION('ref_axis',(1.,0.,0.));
#15904=DIRECTION('center_axis',(0.,0.,1.));
#15905=DIRECTION('ref_axis',(1.,0.,0.));
#15906=DIRECTION('axis',(0.,0.,1.));
#15907=DIRECTION('refdir',(1.,0.,0.));
#15908=DIRECTION('center_axis',(0.,1.,0.));
#15909=DIRECTION('ref_axis',(-1.,0.,0.));
#15910=DIRECTION('',(-1.,0.,0.));
#15911=DIRECTION('',(0.,0.,1.));
#15912=DIRECTION('',(-1.,0.,0.));
#15913=DIRECTION('',(0.,0.,1.));
#15914=DIRECTION('center_axis',(1.,0.,0.));
#15915=DIRECTION('ref_axis',(0.,1.,0.));
#15916=DIRECTION('',(0.,1.,0.));
#15917=DIRECTION('',(0.,1.,0.));
#15918=DIRECTION('',(0.,0.,1.));
#15919=DIRECTION('center_axis',(0.,-1.,0.));
#15920=DIRECTION('ref_axis',(1.,0.,0.));
#15921=DIRECTION('',(1.,0.,0.));
#15922=DIRECTION('',(1.,0.,0.));
#15923=DIRECTION('',(0.,0.,1.));
#15924=DIRECTION('center_axis',(-1.,0.,0.));
#15925=DIRECTION('ref_axis',(0.,-1.,0.));
#15926=DIRECTION('',(0.,-1.,0.));
#15927=DIRECTION('',(0.,-1.,0.));
#15928=DIRECTION('center_axis',(0.,0.,1.));
#15929=DIRECTION('ref_axis',(1.,0.,0.));
#15930=DIRECTION('center_axis',(0.,0.,1.));
#15931=DIRECTION('ref_axis',(1.,0.,0.));
#15932=DIRECTION('axis',(0.,0.,1.));
#15933=DIRECTION('refdir',(1.,0.,0.));
#15934=DIRECTION('center_axis',(0.,0.,1.));
#15935=DIRECTION('ref_axis',(1.,0.,0.));
#15936=DIRECTION('center_axis',(0.,0.,1.));
#15937=DIRECTION('ref_axis',(1.,0.,0.));
#15938=DIRECTION('',(0.,0.,1.));
#15939=DIRECTION('center_axis',(0.,0.,-1.));
#15940=DIRECTION('ref_axis',(1.,0.,0.));
#15941=DIRECTION('center_axis',(0.,0.,1.));
#15942=DIRECTION('ref_axis',(1.,0.,0.));
#15943=DIRECTION('center_axis',(0.,0.,1.));
#15944=DIRECTION('ref_axis',(1.,0.,0.));
#15945=DIRECTION('center_axis',(0.,0.,1.));
#15946=DIRECTION('ref_axis',(1.,0.,0.));
#15947=DIRECTION('center_axis',(0.,0.,1.));
#15948=DIRECTION('ref_axis',(1.,0.,0.));
#15949=DIRECTION('',(0.,0.,1.));
#15950=DIRECTION('center_axis',(0.,0.,-1.));
#15951=DIRECTION('ref_axis',(1.,0.,0.));
#15952=DIRECTION('center_axis',(0.,0.,1.));
#15953=DIRECTION('ref_axis',(1.,0.,0.));
#15954=DIRECTION('center_axis',(0.,0.,1.));
#15955=DIRECTION('ref_axis',(1.,0.,0.));
#15956=DIRECTION('center_axis',(0.,0.,1.));
#15957=DIRECTION('ref_axis',(1.,0.,0.));
#15958=DIRECTION('center_axis',(0.,0.,1.));
#15959=DIRECTION('ref_axis',(1.,0.,0.));
#15960=DIRECTION('',(0.,0.,1.));
#15961=DIRECTION('center_axis',(0.,0.,1.));
#15962=DIRECTION('ref_axis',(1.,0.,0.));
#15963=DIRECTION('center_axis',(0.,0.,1.));
#15964=DIRECTION('ref_axis',(1.,0.,0.));
#15965=DIRECTION('',(0.,0.,1.));
#15966=DIRECTION('center_axis',(0.,1.,0.));
#15967=DIRECTION('ref_axis',(-1.,0.,0.));
#15968=DIRECTION('',(-1.,0.,0.));
#15969=DIRECTION('',(0.,0.,1.));
#15970=DIRECTION('',(-1.,0.,0.));
#15971=DIRECTION('',(0.,0.,1.));
#15972=DIRECTION('center_axis',(1.,0.,0.));
#15973=DIRECTION('ref_axis',(0.,1.,0.));
#15974=DIRECTION('',(0.,1.,0.));
#15975=DIRECTION('',(0.,1.,0.));
#15976=DIRECTION('',(0.,0.,1.));
#15977=DIRECTION('center_axis',(0.,-1.,0.));
#15978=DIRECTION('ref_axis',(1.,0.,0.));
#15979=DIRECTION('',(1.,0.,0.));
#15980=DIRECTION('',(1.,0.,0.));
#15981=DIRECTION('',(0.,0.,1.));
#15982=DIRECTION('center_axis',(-1.,0.,0.));
#15983=DIRECTION('ref_axis',(0.,-1.,0.));
#15984=DIRECTION('',(0.,-1.,0.));
#15985=DIRECTION('',(0.,-1.,0.));
#15986=DIRECTION('center_axis',(0.,0.,1.));
#15987=DIRECTION('ref_axis',(1.,0.,0.));
#15988=DIRECTION('center_axis',(0.,0.,1.));
#15989=DIRECTION('ref_axis',(1.,0.,0.));
#15990=DIRECTION('axis',(0.,0.,1.));
#15991=DIRECTION('refdir',(1.,0.,0.));
#15992=DIRECTION('center_axis',(0.,1.,0.));
#15993=DIRECTION('ref_axis',(-1.,0.,0.));
#15994=DIRECTION('',(-1.,0.,0.));
#15995=DIRECTION('',(0.,0.,1.));
#15996=DIRECTION('',(-1.,0.,0.));
#15997=DIRECTION('',(0.,0.,1.));
#15998=DIRECTION('center_axis',(1.,0.,0.));
#15999=DIRECTION('ref_axis',(0.,1.,0.));
#16000=DIRECTION('',(0.,1.,0.));
#16001=DIRECTION('',(0.,1.,0.));
#16002=DIRECTION('',(0.,0.,1.));
#16003=DIRECTION('center_axis',(0.,-1.,0.));
#16004=DIRECTION('ref_axis',(1.,0.,0.));
#16005=DIRECTION('',(1.,0.,0.));
#16006=DIRECTION('',(1.,0.,0.));
#16007=DIRECTION('',(0.,0.,1.));
#16008=DIRECTION('center_axis',(-1.,0.,0.));
#16009=DIRECTION('ref_axis',(0.,-1.,0.));
#16010=DIRECTION('',(0.,-1.,0.));
#16011=DIRECTION('',(0.,-1.,0.));
#16012=DIRECTION('center_axis',(0.,0.,1.));
#16013=DIRECTION('ref_axis',(1.,0.,0.));
#16014=DIRECTION('center_axis',(0.,0.,1.));
#16015=DIRECTION('ref_axis',(1.,0.,0.));
#16016=DIRECTION('axis',(0.,0.,1.));
#16017=DIRECTION('refdir',(1.,0.,0.));
#16018=DIRECTION('center_axis',(0.,0.,1.));
#16019=DIRECTION('ref_axis',(1.,0.,0.));
#16020=DIRECTION('center_axis',(0.,0.,1.));
#16021=DIRECTION('ref_axis',(1.,0.,0.));
#16022=DIRECTION('',(0.,0.,1.));
#16023=DIRECTION('center_axis',(0.,0.,-1.));
#16024=DIRECTION('ref_axis',(1.,0.,0.));
#16025=DIRECTION('center_axis',(0.,0.,1.));
#16026=DIRECTION('ref_axis',(1.,0.,0.));
#16027=DIRECTION('center_axis',(0.,0.,1.));
#16028=DIRECTION('ref_axis',(1.,0.,0.));
#16029=DIRECTION('',(0.,0.,1.));
#16030=DIRECTION('center_axis',(0.,0.,-1.));
#16031=DIRECTION('ref_axis',(1.,0.,0.));
#16032=DIRECTION('center_axis',(0.,1.,0.));
#16033=DIRECTION('ref_axis',(1.,0.,0.));
#16034=DIRECTION('center_axis',(0.,1.,0.));
#16035=DIRECTION('ref_axis',(1.,0.,0.));
#16036=DIRECTION('',(0.,1.,0.));
#16037=DIRECTION('center_axis',(0.,-1.,0.));
#16038=DIRECTION('ref_axis',(1.,0.,0.));
#16039=DIRECTION('center_axis',(0.,1.,0.));
#16040=DIRECTION('ref_axis',(1.,0.,0.));
#16041=DIRECTION('center_axis',(0.,1.,0.));
#16042=DIRECTION('ref_axis',(1.,0.,0.));
#16043=DIRECTION('',(0.,1.,0.));
#16044=DIRECTION('center_axis',(0.,-1.,0.));
#16045=DIRECTION('ref_axis',(1.,0.,0.));
#16046=DIRECTION('center_axis',(0.,1.,0.));
#16047=DIRECTION('ref_axis',(1.,0.,0.));
#16048=DIRECTION('center_axis',(0.,1.,0.));
#16049=DIRECTION('ref_axis',(1.,0.,0.));
#16050=DIRECTION('',(0.,1.,0.));
#16051=DIRECTION('center_axis',(0.,-1.,0.));
#16052=DIRECTION('ref_axis',(1.,0.,0.));
#16053=DIRECTION('center_axis',(0.,1.,0.));
#16054=DIRECTION('ref_axis',(1.,0.,0.));
#16055=DIRECTION('center_axis',(0.,1.,0.));
#16056=DIRECTION('ref_axis',(1.,0.,0.));
#16057=DIRECTION('',(0.,1.,0.));
#16058=DIRECTION('center_axis',(0.,-1.,0.));
#16059=DIRECTION('ref_axis',(1.,0.,0.));
#16060=DIRECTION('center_axis',(0.,1.,0.));
#16061=DIRECTION('ref_axis',(1.,0.,0.));
#16062=DIRECTION('center_axis',(0.,1.,0.));
#16063=DIRECTION('ref_axis',(1.,0.,0.));
#16064=DIRECTION('',(0.,1.,0.));
#16065=DIRECTION('center_axis',(0.,-1.,0.));
#16066=DIRECTION('ref_axis',(1.,0.,0.));
#16067=DIRECTION('center_axis',(0.,0.,1.));
#16068=DIRECTION('ref_axis',(1.,0.,0.));
#16069=DIRECTION('',(0.,1.,0.));
#16070=DIRECTION('',(-1.,0.,0.));
#16071=DIRECTION('',(0.,1.,0.));
#16072=DIRECTION('',(1.,0.,0.));
#16073=DIRECTION('center_axis',(0.,0.,1.));
#16074=DIRECTION('ref_axis',(1.,0.,0.));
#16075=DIRECTION('',(0.,-1.,0.));
#16076=DIRECTION('',(1.,0.,0.));
#16077=DIRECTION('',(0.,1.,0.));
#16078=DIRECTION('',(-1.,0.,0.));
#16079=DIRECTION('center_axis',(-1.,0.,0.));
#16080=DIRECTION('ref_axis',(0.,0.,1.));
#16081=DIRECTION('',(0.,0.,-1.));
#16082=DIRECTION('',(0.,0.,1.));
#16083=DIRECTION('',(0.,1.,0.));
#16084=DIRECTION('center_axis',(1.,0.,0.));
#16085=DIRECTION('ref_axis',(0.,0.,-1.));
#16086=DIRECTION('',(0.,0.,1.));
#16087=DIRECTION('',(0.,1.,0.));
#16088=DIRECTION('',(0.,0.,-1.));
#16089=DIRECTION('center_axis',(0.,-1.,0.));
#16090=DIRECTION('ref_axis',(1.,0.,0.));
#16091=DIRECTION('',(0.,0.,1.));
#16092=DIRECTION('',(1.,0.,0.));
#16093=DIRECTION('',(0.,0.,1.));
#16094=DIRECTION('',(1.,0.,0.));
#16095=DIRECTION('center_axis',(1.,0.,0.));
#16096=DIRECTION('ref_axis',(0.,1.,0.));
#16097=DIRECTION('',(0.,0.,1.));
#16098=DIRECTION('',(0.,1.,0.));
#16099=DIRECTION('center_axis',(0.,1.,0.));
#16100=DIRECTION('ref_axis',(-1.,0.,0.));
#16101=DIRECTION('',(0.,0.,1.));
#16102=DIRECTION('',(-1.,0.,0.));
#16103=DIRECTION('',(-1.,0.,0.));
#16104=DIRECTION('center_axis',(-1.,0.,0.));
#16105=DIRECTION('ref_axis',(0.,-1.,0.));
#16106=DIRECTION('',(0.,-1.,0.));
#16107=DIRECTION('center_axis',(0.,0.,1.));
#16108=DIRECTION('ref_axis',(1.,0.,0.));
#16109=DIRECTION('center_axis',(0.,0.,1.));
#16110=DIRECTION('ref_axis',(1.,0.,0.));
#16111=DIRECTION('axis',(0.,0.,1.));
#16112=DIRECTION('refdir',(1.,0.,0.));
#16113=DIRECTION('center_axis',(0.,1.,0.));
#16114=DIRECTION('ref_axis',(1.,0.,0.));
#16115=DIRECTION('center_axis',(0.,1.,0.));
#16116=DIRECTION('ref_axis',(1.,0.,0.));
#16117=DIRECTION('',(0.,1.,0.));
#16118=DIRECTION('center_axis',(0.,-1.,0.));
#16119=DIRECTION('ref_axis',(1.,0.,0.));
#16120=DIRECTION('center_axis',(0.,1.,0.));
#16121=DIRECTION('ref_axis',(1.,0.,0.));
#16122=DIRECTION('center_axis',(0.,1.,0.));
#16123=DIRECTION('ref_axis',(1.,0.,0.));
#16124=DIRECTION('',(0.,1.,0.));
#16125=DIRECTION('center_axis',(0.,-1.,0.));
#16126=DIRECTION('ref_axis',(1.,0.,0.));
#16127=DIRECTION('center_axis',(0.,1.,0.));
#16128=DIRECTION('ref_axis',(1.,0.,0.));
#16129=DIRECTION('center_axis',(0.,1.,0.));
#16130=DIRECTION('ref_axis',(1.,0.,0.));
#16131=DIRECTION('',(0.,1.,0.));
#16132=DIRECTION('center_axis',(0.,-1.,0.));
#16133=DIRECTION('ref_axis',(1.,0.,0.));
#16134=DIRECTION('center_axis',(0.,1.,0.));
#16135=DIRECTION('ref_axis',(1.,0.,0.));
#16136=DIRECTION('center_axis',(0.,1.,0.));
#16137=DIRECTION('ref_axis',(1.,0.,0.));
#16138=DIRECTION('',(0.,1.,0.));
#16139=DIRECTION('center_axis',(0.,-1.,0.));
#16140=DIRECTION('ref_axis',(1.,0.,0.));
#16141=DIRECTION('center_axis',(0.,1.,0.));
#16142=DIRECTION('ref_axis',(1.,0.,0.));
#16143=DIRECTION('center_axis',(0.,1.,0.));
#16144=DIRECTION('ref_axis',(1.,0.,0.));
#16145=DIRECTION('',(0.,-1.,0.));
#16146=DIRECTION('center_axis',(0.,-1.,0.));
#16147=DIRECTION('ref_axis',(1.,0.,0.));
#16148=DIRECTION('center_axis',(0.,1.,0.));
#16149=DIRECTION('ref_axis',(1.,0.,0.));
#16150=DIRECTION('center_axis',(0.,-1.,0.));
#16151=DIRECTION('ref_axis',(1.,0.,0.));
#16152=DIRECTION('center_axis',(0.,1.,0.));
#16153=DIRECTION('ref_axis',(1.,0.,0.));
#16154=DIRECTION('',(0.,-1.,0.));
#16155=DIRECTION('center_axis',(0.,-1.,0.));
#16156=DIRECTION('ref_axis',(1.,0.,0.));
#16157=DIRECTION('center_axis',(0.,1.,0.));
#16158=DIRECTION('ref_axis',(1.,0.,0.));
#16159=DIRECTION('center_axis',(0.,1.,0.));
#16160=DIRECTION('ref_axis',(1.,0.,0.));
#16161=DIRECTION('',(0.,-1.,0.));
#16162=DIRECTION('center_axis',(0.,1.,0.));
#16163=DIRECTION('ref_axis',(1.,0.,0.));
#16164=DIRECTION('center_axis',(0.,1.,0.));
#16165=DIRECTION('ref_axis',(1.,0.,0.));
#16166=DIRECTION('center_axis',(0.,1.,0.));
#16167=DIRECTION('ref_axis',(1.,0.,0.));
#16168=DIRECTION('axis',(0.,0.,1.));
#16169=DIRECTION('refdir',(1.,0.,0.));
#16170=DIRECTION('center_axis',(0.,1.,0.));
#16171=DIRECTION('ref_axis',(1.,0.,0.));
#16172=DIRECTION('center_axis',(0.,1.,0.));
#16173=DIRECTION('ref_axis',(1.,0.,0.));
#16174=DIRECTION('',(0.,1.,0.));
#16175=DIRECTION('center_axis',(0.,-1.,0.));
#16176=DIRECTION('ref_axis',(1.,0.,0.));
#16177=DIRECTION('center_axis',(0.,1.,0.));
#16178=DIRECTION('ref_axis',(1.,0.,0.));
#16179=DIRECTION('center_axis',(0.,1.,0.));
#16180=DIRECTION('ref_axis',(1.,0.,0.));
#16181=DIRECTION('',(0.,1.,0.));
#16182=DIRECTION('center_axis',(0.,-1.,0.));
#16183=DIRECTION('ref_axis',(1.,0.,0.));
#16184=DIRECTION('center_axis',(0.,1.,0.));
#16185=DIRECTION('ref_axis',(1.,0.,0.));
#16186=DIRECTION('center_axis',(0.,1.,0.));
#16187=DIRECTION('ref_axis',(1.,0.,0.));
#16188=DIRECTION('',(0.,1.,0.));
#16189=DIRECTION('center_axis',(0.,-1.,0.));
#16190=DIRECTION('ref_axis',(1.,0.,0.));
#16191=DIRECTION('center_axis',(0.,1.,0.));
#16192=DIRECTION('ref_axis',(1.,0.,0.));
#16193=DIRECTION('center_axis',(0.,1.,0.));
#16194=DIRECTION('ref_axis',(1.,0.,0.));
#16195=DIRECTION('',(0.,1.,0.));
#16196=DIRECTION('center_axis',(0.,-1.,0.));
#16197=DIRECTION('ref_axis',(1.,0.,0.));
#16198=DIRECTION('center_axis',(0.,1.,0.));
#16199=DIRECTION('ref_axis',(1.,0.,0.));
#16200=DIRECTION('center_axis',(0.,1.,0.));
#16201=DIRECTION('ref_axis',(1.,0.,0.));
#16202=DIRECTION('',(0.,-1.,0.));
#16203=DIRECTION('center_axis',(0.,1.,0.));
#16204=DIRECTION('ref_axis',(1.,0.,0.));
#16205=DIRECTION('center_axis',(0.,1.,0.));
#16206=DIRECTION('ref_axis',(1.,0.,0.));
#16207=DIRECTION('center_axis',(0.,-1.,0.));
#16208=DIRECTION('ref_axis',(1.,0.,0.));
#16209=DIRECTION('center_axis',(0.,1.,0.));
#16210=DIRECTION('ref_axis',(1.,0.,0.));
#16211=DIRECTION('center_axis',(0.,-1.,0.));
#16212=DIRECTION('ref_axis',(1.,0.,0.));
#16213=DIRECTION('',(0.,-1.,0.));
#16214=DIRECTION('center_axis',(0.,1.,0.));
#16215=DIRECTION('ref_axis',(1.,0.,0.));
#16216=DIRECTION('center_axis',(0.,1.,0.));
#16217=DIRECTION('ref_axis',(1.,0.,0.));
#16218=DIRECTION('',(0.,-1.,0.));
#16219=DIRECTION('center_axis',(0.,1.,0.));
#16220=DIRECTION('ref_axis',(1.,0.,0.));
#16221=DIRECTION('center_axis',(0.,1.,0.));
#16222=DIRECTION('ref_axis',(1.,0.,0.));
#16223=DIRECTION('center_axis',(0.,1.,0.));
#16224=DIRECTION('ref_axis',(1.,0.,0.));
#16225=DIRECTION('axis',(0.,0.,1.));
#16226=DIRECTION('refdir',(1.,0.,0.));
#16227=DIRECTION('center_axis',(0.,0.,1.));
#16228=DIRECTION('ref_axis',(1.,0.,0.));
#16229=DIRECTION('center_axis',(0.,0.,1.));
#16230=DIRECTION('ref_axis',(1.,0.,0.));
#16231=DIRECTION('',(0.,0.,1.));
#16232=DIRECTION('center_axis',(0.,0.,-1.));
#16233=DIRECTION('ref_axis',(1.,0.,0.));
#16234=DIRECTION('center_axis',(0.,0.,1.));
#16235=DIRECTION('ref_axis',(1.,0.,0.));
#16236=DIRECTION('center_axis',(0.,0.,1.));
#16237=DIRECTION('ref_axis',(1.,0.,0.));
#16238=DIRECTION('',(0.,0.,1.));
#16239=DIRECTION('center_axis',(0.,0.,-1.));
#16240=DIRECTION('ref_axis',(1.,0.,0.));
#16241=DIRECTION('center_axis',(0.,1.,0.));
#16242=DIRECTION('ref_axis',(1.,0.,0.));
#16243=DIRECTION('center_axis',(0.,1.,0.));
#16244=DIRECTION('ref_axis',(1.,0.,0.));
#16245=DIRECTION('',(0.,1.,0.));
#16246=DIRECTION('center_axis',(0.,-1.,0.));
#16247=DIRECTION('ref_axis',(1.,0.,0.));
#16248=DIRECTION('center_axis',(0.,1.,0.));
#16249=DIRECTION('ref_axis',(1.,0.,0.));
#16250=DIRECTION('center_axis',(0.,1.,0.));
#16251=DIRECTION('ref_axis',(1.,0.,0.));
#16252=DIRECTION('',(0.,1.,0.));
#16253=DIRECTION('center_axis',(0.,-1.,0.));
#16254=DIRECTION('ref_axis',(1.,0.,0.));
#16255=DIRECTION('center_axis',(0.,1.,0.));
#16256=DIRECTION('ref_axis',(1.,0.,0.));
#16257=DIRECTION('center_axis',(0.,1.,0.));
#16258=DIRECTION('ref_axis',(1.,0.,0.));
#16259=DIRECTION('',(0.,1.,0.));
#16260=DIRECTION('center_axis',(0.,-1.,0.));
#16261=DIRECTION('ref_axis',(1.,0.,0.));
#16262=DIRECTION('center_axis',(0.,1.,0.));
#16263=DIRECTION('ref_axis',(1.,0.,0.));
#16264=DIRECTION('center_axis',(0.,1.,0.));
#16265=DIRECTION('ref_axis',(1.,0.,0.));
#16266=DIRECTION('',(0.,1.,0.));
#16267=DIRECTION('center_axis',(0.,-1.,0.));
#16268=DIRECTION('ref_axis',(1.,0.,0.));
#16269=DIRECTION('center_axis',(0.,1.,0.));
#16270=DIRECTION('ref_axis',(1.,0.,0.));
#16271=DIRECTION('center_axis',(0.,1.,0.));
#16272=DIRECTION('ref_axis',(1.,0.,0.));
#16273=DIRECTION('',(0.,1.,0.));
#16274=DIRECTION('center_axis',(0.,-1.,0.));
#16275=DIRECTION('ref_axis',(1.,0.,0.));
#16276=DIRECTION('center_axis',(0.,0.,1.));
#16277=DIRECTION('ref_axis',(1.,0.,0.));
#16278=DIRECTION('',(0.,1.,0.));
#16279=DIRECTION('',(-1.,0.,0.));
#16280=DIRECTION('',(0.,1.,0.));
#16281=DIRECTION('',(1.,0.,0.));
#16282=DIRECTION('center_axis',(0.,0.,1.));
#16283=DIRECTION('ref_axis',(1.,0.,0.));
#16284=DIRECTION('',(0.,-1.,0.));
#16285=DIRECTION('',(1.,0.,0.));
#16286=DIRECTION('',(0.,1.,0.));
#16287=DIRECTION('',(-1.,0.,0.));
#16288=DIRECTION('center_axis',(-1.,0.,0.));
#16289=DIRECTION('ref_axis',(0.,0.,1.));
#16290=DIRECTION('',(0.,0.,-1.));
#16291=DIRECTION('',(0.,0.,1.));
#16292=DIRECTION('',(0.,1.,0.));
#16293=DIRECTION('center_axis',(1.,0.,0.));
#16294=DIRECTION('ref_axis',(0.,0.,-1.));
#16295=DIRECTION('',(0.,0.,1.));
#16296=DIRECTION('',(0.,1.,0.));
#16297=DIRECTION('',(0.,0.,-1.));
#16298=DIRECTION('center_axis',(0.,-1.,0.));
#16299=DIRECTION('ref_axis',(1.,0.,0.));
#16300=DIRECTION('',(0.,0.,1.));
#16301=DIRECTION('',(1.,0.,0.));
#16302=DIRECTION('',(0.,0.,1.));
#16303=DIRECTION('',(1.,0.,0.));
#16304=DIRECTION('center_axis',(1.,0.,0.));
#16305=DIRECTION('ref_axis',(0.,1.,0.));
#16306=DIRECTION('',(0.,0.,1.));
#16307=DIRECTION('',(0.,1.,0.));
#16308=DIRECTION('center_axis',(0.,1.,0.));
#16309=DIRECTION('ref_axis',(-1.,0.,0.));
#16310=DIRECTION('',(0.,0.,1.));
#16311=DIRECTION('',(-1.,0.,0.));
#16312=DIRECTION('',(-1.,0.,0.));
#16313=DIRECTION('center_axis',(-1.,0.,0.));
#16314=DIRECTION('ref_axis',(0.,-1.,0.));
#16315=DIRECTION('',(0.,-1.,0.));
#16316=DIRECTION('center_axis',(0.,0.,1.));
#16317=DIRECTION('ref_axis',(1.,0.,0.));
#16318=DIRECTION('center_axis',(0.,0.,1.));
#16319=DIRECTION('ref_axis',(1.,0.,0.));
#16320=DIRECTION('axis',(0.,0.,1.));
#16321=DIRECTION('refdir',(1.,0.,0.));
#16322=DIRECTION('center_axis',(0.,1.,0.));
#16323=DIRECTION('ref_axis',(1.,0.,0.));
#16324=DIRECTION('center_axis',(0.,1.,0.));
#16325=DIRECTION('ref_axis',(1.,0.,0.));
#16326=DIRECTION('',(0.,1.,0.));
#16327=DIRECTION('center_axis',(0.,-1.,0.));
#16328=DIRECTION('ref_axis',(1.,0.,0.));
#16329=DIRECTION('center_axis',(0.,1.,0.));
#16330=DIRECTION('ref_axis',(1.,0.,0.));
#16331=DIRECTION('center_axis',(0.,1.,0.));
#16332=DIRECTION('ref_axis',(1.,0.,0.));
#16333=DIRECTION('',(0.,1.,0.));
#16334=DIRECTION('center_axis',(0.,-1.,0.));
#16335=DIRECTION('ref_axis',(1.,0.,0.));
#16336=DIRECTION('center_axis',(0.,1.,0.));
#16337=DIRECTION('ref_axis',(1.,0.,0.));
#16338=DIRECTION('center_axis',(0.,1.,0.));
#16339=DIRECTION('ref_axis',(1.,0.,0.));
#16340=DIRECTION('',(0.,1.,0.));
#16341=DIRECTION('center_axis',(0.,-1.,0.));
#16342=DIRECTION('ref_axis',(1.,0.,0.));
#16343=DIRECTION('center_axis',(0.,1.,0.));
#16344=DIRECTION('ref_axis',(1.,0.,0.));
#16345=DIRECTION('center_axis',(0.,1.,0.));
#16346=DIRECTION('ref_axis',(1.,0.,0.));
#16347=DIRECTION('',(0.,1.,0.));
#16348=DIRECTION('center_axis',(0.,-1.,0.));
#16349=DIRECTION('ref_axis',(1.,0.,0.));
#16350=DIRECTION('center_axis',(0.,1.,0.));
#16351=DIRECTION('ref_axis',(1.,0.,0.));
#16352=DIRECTION('center_axis',(0.,1.,0.));
#16353=DIRECTION('ref_axis',(1.,0.,0.));
#16354=DIRECTION('',(0.,-1.,0.));
#16355=DIRECTION('center_axis',(0.,-1.,0.));
#16356=DIRECTION('ref_axis',(1.,0.,0.));
#16357=DIRECTION('center_axis',(0.,1.,0.));
#16358=DIRECTION('ref_axis',(1.,0.,0.));
#16359=DIRECTION('center_axis',(0.,-1.,0.));
#16360=DIRECTION('ref_axis',(1.,0.,0.));
#16361=DIRECTION('center_axis',(0.,1.,0.));
#16362=DIRECTION('ref_axis',(1.,0.,0.));
#16363=DIRECTION('',(0.,-1.,0.));
#16364=DIRECTION('center_axis',(0.,-1.,0.));
#16365=DIRECTION('ref_axis',(1.,0.,0.));
#16366=DIRECTION('center_axis',(0.,1.,0.));
#16367=DIRECTION('ref_axis',(1.,0.,0.));
#16368=DIRECTION('center_axis',(0.,1.,0.));
#16369=DIRECTION('ref_axis',(1.,0.,0.));
#16370=DIRECTION('',(0.,-1.,0.));
#16371=DIRECTION('center_axis',(0.,1.,0.));
#16372=DIRECTION('ref_axis',(1.,0.,0.));
#16373=DIRECTION('center_axis',(0.,1.,0.));
#16374=DIRECTION('ref_axis',(1.,0.,0.));
#16375=DIRECTION('center_axis',(0.,1.,0.));
#16376=DIRECTION('ref_axis',(1.,0.,0.));
#16377=DIRECTION('axis',(0.,0.,1.));
#16378=DIRECTION('refdir',(1.,0.,0.));
#16379=DIRECTION('center_axis',(0.,1.,0.));
#16380=DIRECTION('ref_axis',(1.,0.,0.));
#16381=DIRECTION('center_axis',(0.,1.,0.));
#16382=DIRECTION('ref_axis',(1.,0.,0.));
#16383=DIRECTION('',(0.,1.,0.));
#16384=DIRECTION('center_axis',(0.,-1.,0.));
#16385=DIRECTION('ref_axis',(1.,0.,0.));
#16386=DIRECTION('center_axis',(0.,1.,0.));
#16387=DIRECTION('ref_axis',(1.,0.,0.));
#16388=DIRECTION('center_axis',(0.,1.,0.));
#16389=DIRECTION('ref_axis',(1.,0.,0.));
#16390=DIRECTION('',(0.,1.,0.));
#16391=DIRECTION('center_axis',(0.,-1.,0.));
#16392=DIRECTION('ref_axis',(1.,0.,0.));
#16393=DIRECTION('center_axis',(0.,1.,0.));
#16394=DIRECTION('ref_axis',(1.,0.,0.));
#16395=DIRECTION('center_axis',(0.,1.,0.));
#16396=DIRECTION('ref_axis',(1.,0.,0.));
#16397=DIRECTION('',(0.,1.,0.));
#16398=DIRECTION('center_axis',(0.,-1.,0.));
#16399=DIRECTION('ref_axis',(1.,0.,0.));
#16400=DIRECTION('center_axis',(0.,1.,0.));
#16401=DIRECTION('ref_axis',(1.,0.,0.));
#16402=DIRECTION('center_axis',(0.,1.,0.));
#16403=DIRECTION('ref_axis',(1.,0.,0.));
#16404=DIRECTION('',(0.,1.,0.));
#16405=DIRECTION('center_axis',(0.,-1.,0.));
#16406=DIRECTION('ref_axis',(1.,0.,0.));
#16407=DIRECTION('center_axis',(0.,1.,0.));
#16408=DIRECTION('ref_axis',(1.,0.,0.));
#16409=DIRECTION('center_axis',(0.,1.,0.));
#16410=DIRECTION('ref_axis',(1.,0.,0.));
#16411=DIRECTION('',(0.,-1.,0.));
#16412=DIRECTION('center_axis',(0.,1.,0.));
#16413=DIRECTION('ref_axis',(1.,0.,0.));
#16414=DIRECTION('center_axis',(0.,1.,0.));
#16415=DIRECTION('ref_axis',(1.,0.,0.));
#16416=DIRECTION('center_axis',(0.,-1.,0.));
#16417=DIRECTION('ref_axis',(1.,0.,0.));
#16418=DIRECTION('center_axis',(0.,1.,0.));
#16419=DIRECTION('ref_axis',(1.,0.,0.));
#16420=DIRECTION('center_axis',(0.,-1.,0.));
#16421=DIRECTION('ref_axis',(1.,0.,0.));
#16422=DIRECTION('',(0.,-1.,0.));
#16423=DIRECTION('center_axis',(0.,1.,0.));
#16424=DIRECTION('ref_axis',(1.,0.,0.));
#16425=DIRECTION('center_axis',(0.,1.,0.));
#16426=DIRECTION('ref_axis',(1.,0.,0.));
#16427=DIRECTION('',(0.,-1.,0.));
#16428=DIRECTION('center_axis',(0.,1.,0.));
#16429=DIRECTION('ref_axis',(1.,0.,0.));
#16430=DIRECTION('center_axis',(0.,1.,0.));
#16431=DIRECTION('ref_axis',(1.,0.,0.));
#16432=DIRECTION('center_axis',(0.,1.,0.));
#16433=DIRECTION('ref_axis',(1.,0.,0.));
#16434=DIRECTION('axis',(0.,0.,1.));
#16435=DIRECTION('refdir',(1.,0.,0.));
#16436=DIRECTION('center_axis',(0.,0.,-1.));
#16437=DIRECTION('ref_axis',(0.,1.,0.));
#16438=DIRECTION('',(0.,1.,0.));
#16439=DIRECTION('',(1.,0.,0.));
#16440=DIRECTION('',(0.,-1.,0.));
#16441=DIRECTION('',(1.,0.,0.));
#16442=DIRECTION('center_axis',(0.,1.,-8.88178419700125E-16));
#16443=DIRECTION('ref_axis',(0.,8.88178419700125E-16,1.));
#16444=DIRECTION('',(0.,8.88178419700125E-16,1.));
#16445=DIRECTION('',(1.,0.,0.));
#16446=DIRECTION('',(0.,-8.88178419700125E-16,-1.));
#16447=DIRECTION('center_axis',(0.,-7.40148683083439E-16,-1.));
#16448=DIRECTION('ref_axis',(0.,1.,-7.40148683083439E-16));
#16449=DIRECTION('',(0.,1.,-7.40148683083439E-16));
#16450=DIRECTION('',(1.,0.,0.));
#16451=DIRECTION('',(0.,-1.,7.40148683083439E-16));
#16452=DIRECTION('center_axis',(0.,-0.707106781186547,-0.707106781186548));
#16453=DIRECTION('ref_axis',(0.,0.707106781186548,-0.707106781186547));
#16454=DIRECTION('',(0.,0.707106781186548,-0.707106781186547));
#16455=DIRECTION('',(1.,0.,0.));
#16456=DIRECTION('',(0.,-0.707106781186548,0.707106781186547));
#16457=DIRECTION('center_axis',(0.,-1.,2.77555756156289E-16));
#16458=DIRECTION('ref_axis',(0.,-2.77555756156289E-16,-1.));
#16459=DIRECTION('',(0.,-2.77555756156289E-16,-1.));
#16460=DIRECTION('',(1.,0.,0.));
#16461=DIRECTION('',(0.,2.77555756156289E-16,1.));
#16462=DIRECTION('center_axis',(0.,-0.707106781186547,0.707106781186548));
#16463=DIRECTION('ref_axis',(0.,-0.707106781186548,-0.707106781186547));
#16464=DIRECTION('',(0.,-0.707106781186548,-0.707106781186547));
#16465=DIRECTION('',(1.,0.,0.));
#16466=DIRECTION('',(0.,0.707106781186548,0.707106781186547));
#16467=DIRECTION('center_axis',(0.,7.40148683083438E-16,1.));
#16468=DIRECTION('ref_axis',(0.,-1.,7.40148683083438E-16));
#16469=DIRECTION('',(0.,-1.,7.40148683083438E-16));
#16470=DIRECTION('',(1.,0.,0.));
#16471=DIRECTION('',(0.,1.,-7.40148683083438E-16));
#16472=DIRECTION('center_axis',(0.,1.,-4.44089209850063E-16));
#16473=DIRECTION('ref_axis',(0.,4.44089209850063E-16,1.));
#16474=DIRECTION('',(0.,4.44089209850063E-16,1.));
#16475=DIRECTION('',(1.,0.,0.));
#16476=DIRECTION('',(0.,-4.44089209850063E-16,-1.));
#16477=DIRECTION('center_axis',(0.,2.41352831440251E-16,1.));
#16478=DIRECTION('ref_axis',(0.,-1.,2.41352831440251E-16));
#16479=DIRECTION('',(0.,-1.,2.41352831440251E-16));
#16480=DIRECTION('',(-1.,0.,0.));
#16481=DIRECTION('',(0.,1.,-2.41352831440251E-16));
#16482=DIRECTION('center_axis',(0.,-1.,2.41352831440251E-16));
#16483=DIRECTION('ref_axis',(0.,-2.41352831440251E-16,-1.));
#16484=DIRECTION('',(0.,-2.41352831440251E-16,-1.));
#16485=DIRECTION('',(1.,0.,0.));
#16486=DIRECTION('',(0.,2.41352831440251E-16,1.));
#16487=DIRECTION('',(1.,0.,0.));
#16488=DIRECTION('center_axis',(0.,0.,-1.));
#16489=DIRECTION('ref_axis',(0.,1.,0.));
#16490=DIRECTION('',(0.,1.,0.));
#16491=DIRECTION('',(1.,0.,0.));
#16492=DIRECTION('',(0.,-1.,0.));
#16493=DIRECTION('center_axis',(0.,-1.,0.));
#16494=DIRECTION('ref_axis',(0.,0.,-1.));
#16495=DIRECTION('',(0.,0.,-1.));
#16496=DIRECTION('',(1.,0.,0.));
#16497=DIRECTION('',(0.,0.,1.));
#16498=DIRECTION('center_axis',(0.,-0.707106781186547,0.707106781186548));
#16499=DIRECTION('ref_axis',(0.,-0.707106781186548,-0.707106781186547));
#16500=DIRECTION('',(0.,-0.707106781186548,-0.707106781186547));
#16501=DIRECTION('',(1.,0.,0.));
#16502=DIRECTION('',(0.,0.707106781186548,0.707106781186547));
#16503=DIRECTION('center_axis',(0.,0.,1.));
#16504=DIRECTION('ref_axis',(0.,-1.,0.));
#16505=DIRECTION('',(0.,-1.,0.));
#16506=DIRECTION('',(1.,0.,0.));
#16507=DIRECTION('',(0.,1.,0.));
#16508=DIRECTION('center_axis',(0.,0.707106781186548,0.707106781186547));
#16509=DIRECTION('ref_axis',(0.,-0.707106781186547,0.707106781186548));
#16510=DIRECTION('',(0.,-0.707106781186547,0.707106781186548));
#16511=DIRECTION('',(1.,0.,0.));
#16512=DIRECTION('',(0.,0.707106781186547,-0.707106781186548));
#16513=DIRECTION('center_axis',(0.,1.,0.));
#16514=DIRECTION('ref_axis',(0.,0.,1.));
#16515=DIRECTION('',(0.,0.,1.));
#16516=DIRECTION('',(1.,0.,0.));
#16517=DIRECTION('',(0.,0.,-1.));
#16518=DIRECTION('center_axis',(0.,0.,-1.));
#16519=DIRECTION('ref_axis',(0.,1.,0.));
#16520=DIRECTION('',(0.,1.,0.));
#16521=DIRECTION('',(1.,0.,0.));
#16522=DIRECTION('',(0.,-1.,0.));
#16523=DIRECTION('center_axis',(0.,1.,-2.41352831440251E-16));
#16524=DIRECTION('ref_axis',(0.,2.41352831440251E-16,1.));
#16525=DIRECTION('',(0.,2.41352831440251E-16,1.));
#16526=DIRECTION('',(-1.,0.,0.));
#16527=DIRECTION('',(0.,-2.41352831440251E-16,-1.));
#16528=DIRECTION('center_axis',(0.,0.,1.));
#16529=DIRECTION('ref_axis',(0.,-1.,0.));
#16530=DIRECTION('',(0.,-1.,0.));
#16531=DIRECTION('',(1.,0.,0.));
#16532=DIRECTION('',(0.,1.,0.));
#16533=DIRECTION('',(1.,0.,0.));
#16534=DIRECTION('center_axis',(0.,-1.,0.));
#16535=DIRECTION('ref_axis',(0.,0.,-1.));
#16536=DIRECTION('',(0.,0.,-1.));
#16537=DIRECTION('',(1.,0.,0.));
#16538=DIRECTION('',(0.,0.,1.));
#16539=DIRECTION('center_axis',(0.,0.,1.));
#16540=DIRECTION('ref_axis',(0.,-1.,0.));
#16541=DIRECTION('',(0.,-1.,0.));
#16542=DIRECTION('',(1.,0.,0.));
#16543=DIRECTION('',(0.,1.,0.));
#16544=DIRECTION('center_axis',(0.,0.707106781186548,0.707106781186548));
#16545=DIRECTION('ref_axis',(0.,-0.707106781186548,0.707106781186548));
#16546=DIRECTION('',(0.,-0.707106781186548,0.707106781186548));
#16547=DIRECTION('',(1.,0.,0.));
#16548=DIRECTION('',(0.,0.707106781186548,-0.707106781186548));
#16549=DIRECTION('center_axis',(0.,1.,0.));
#16550=DIRECTION('ref_axis',(0.,0.,1.));
#16551=DIRECTION('',(0.,0.,1.));
#16552=DIRECTION('',(1.,0.,0.));
#16553=DIRECTION('',(0.,0.,-1.));
#16554=DIRECTION('center_axis',(0.,0.707106781186548,-0.707106781186547));
#16555=DIRECTION('ref_axis',(0.,0.707106781186547,0.707106781186548));
#16556=DIRECTION('',(0.,0.707106781186547,0.707106781186548));
#16557=DIRECTION('',(1.,0.,0.));
#16558=DIRECTION('',(0.,-0.707106781186547,-0.707106781186548));
#16559=DIRECTION('center_axis',(0.,-7.40148683083438E-16,-1.));
#16560=DIRECTION('ref_axis',(0.,1.,-7.40148683083438E-16));
#16561=DIRECTION('',(0.,1.,-7.40148683083438E-16));
#16562=DIRECTION('',(1.,0.,0.));
#16563=DIRECTION('',(0.,-1.,7.40148683083438E-16));
#16564=DIRECTION('center_axis',(0.,-1.,0.));
#16565=DIRECTION('ref_axis',(0.,0.,-1.));
#16566=DIRECTION('',(0.,0.,-1.));
#16567=DIRECTION('',(1.,0.,0.));
#16568=DIRECTION('',(0.,0.,1.));
#16569=DIRECTION('center_axis',(0.,0.,-1.));
#16570=DIRECTION('ref_axis',(0.,1.,0.));
#16571=DIRECTION('',(0.,1.,0.));
#16572=DIRECTION('',(-1.,0.,0.));
#16573=DIRECTION('',(0.,-1.,0.));
#16574=DIRECTION('center_axis',(0.,1.,0.));
#16575=DIRECTION('ref_axis',(0.,0.,1.));
#16576=DIRECTION('',(0.,0.,1.));
#16577=DIRECTION('',(1.,0.,0.));
#16578=DIRECTION('',(0.,0.,-1.));
#16579=DIRECTION('',(1.,0.,0.));
#16580=DIRECTION('center_axis',(0.,0.,1.));
#16581=DIRECTION('ref_axis',(0.,-1.,0.));
#16582=DIRECTION('',(0.,-1.,0.));
#16583=DIRECTION('',(1.,0.,0.));
#16584=DIRECTION('',(0.,1.,0.));
#16585=DIRECTION('center_axis',(0.,1.,0.));
#16586=DIRECTION('ref_axis',(0.,0.,1.));
#16587=DIRECTION('',(0.,0.,1.));
#16588=DIRECTION('',(1.,0.,0.));
#16589=DIRECTION('',(0.,0.,-1.));
#16590=DIRECTION('center_axis',(0.,0.707106781186547,-0.707106781186548));
#16591=DIRECTION('ref_axis',(0.,0.707106781186548,0.707106781186547));
#16592=DIRECTION('',(0.,0.707106781186548,0.707106781186547));
#16593=DIRECTION('',(1.,0.,0.));
#16594=DIRECTION('',(0.,-0.707106781186548,-0.707106781186547));
#16595=DIRECTION('center_axis',(0.,0.,-1.));
#16596=DIRECTION('ref_axis',(0.,1.,0.));
#16597=DIRECTION('',(0.,1.,0.));
#16598=DIRECTION('',(1.,0.,0.));
#16599=DIRECTION('',(0.,-1.,0.));
#16600=DIRECTION('center_axis',(0.,-0.707106781186547,-0.707106781186548));
#16601=DIRECTION('ref_axis',(0.,0.707106781186548,-0.707106781186547));
#16602=DIRECTION('',(0.,0.707106781186548,-0.707106781186547));
#16603=DIRECTION('',(1.,0.,0.));
#16604=DIRECTION('',(0.,-0.707106781186548,0.707106781186547));
#16605=DIRECTION('center_axis',(0.,-1.,0.));
#16606=DIRECTION('ref_axis',(0.,0.,-1.));
#16607=DIRECTION('',(0.,0.,-1.));
#16608=DIRECTION('',(1.,0.,0.));
#16609=DIRECTION('',(0.,0.,1.));
#16610=DIRECTION('center_axis',(0.,0.,1.));
#16611=DIRECTION('ref_axis',(0.,-1.,0.));
#16612=DIRECTION('',(0.,-1.,0.));
#16613=DIRECTION('',(1.,0.,0.));
#16614=DIRECTION('',(0.,1.,0.));
#16615=DIRECTION('center_axis',(0.,-1.,0.));
#16616=DIRECTION('ref_axis',(0.,0.,-1.));
#16617=DIRECTION('',(0.,0.,-1.));
#16618=DIRECTION('',(-1.,0.,0.));
#16619=DIRECTION('',(0.,0.,1.));
#16620=DIRECTION('center_axis',(1.,0.,0.));
#16621=DIRECTION('ref_axis',(0.,0.,-1.));
#16622=DIRECTION('center_axis',(1.,0.,0.));
#16623=DIRECTION('ref_axis',(0.,0.,-1.));
#16624=DIRECTION('',(1.,0.,0.));
#16625=DIRECTION('center_axis',(-1.,0.,0.));
#16626=DIRECTION('ref_axis',(0.,0.,-1.));
#16627=DIRECTION('center_axis',(0.,1.,0.));
#16628=DIRECTION('ref_axis',(0.,0.,1.));
#16629=DIRECTION('',(0.,0.,1.));
#16630=DIRECTION('',(1.,0.,0.));
#16631=DIRECTION('',(0.,0.,1.));
#16632=DIRECTION('center_axis',(0.,1.,0.));
#16633=DIRECTION('ref_axis',(0.,0.,1.));
#16634=DIRECTION('',(0.,0.,1.));
#16635=DIRECTION('',(1.,0.,0.));
#16636=DIRECTION('',(0.,0.,1.));
#16637=DIRECTION('center_axis',(0.,0.,-1.));
#16638=DIRECTION('ref_axis',(0.,1.,0.));
#16639=DIRECTION('',(0.,1.,0.));
#16640=DIRECTION('',(0.,1.,0.));
#16641=DIRECTION('center_axis',(0.,0.,-1.));
#16642=DIRECTION('ref_axis',(0.,1.,0.));
#16643=DIRECTION('',(0.,1.,0.));
#16644=DIRECTION('',(1.,0.,0.));
#16645=DIRECTION('',(0.,1.,0.));
#16646=DIRECTION('center_axis',(0.,-1.,0.));
#16647=DIRECTION('ref_axis',(0.,0.,-1.));
#16648=DIRECTION('',(0.,0.,-1.));
#16649=DIRECTION('',(0.,0.,-1.));
#16650=DIRECTION('center_axis',(0.,-1.,0.));
#16651=DIRECTION('ref_axis',(0.,0.,-1.));
#16652=DIRECTION('',(0.,0.,-1.));
#16653=DIRECTION('',(1.,0.,0.));
#16654=DIRECTION('',(0.,0.,-1.));
#16655=DIRECTION('center_axis',(0.,0.,1.));
#16656=DIRECTION('ref_axis',(0.,-1.,0.));
#16657=DIRECTION('',(0.,-1.,0.));
#16658=DIRECTION('',(0.,-1.,0.));
#16659=DIRECTION('center_axis',(0.,0.,1.));
#16660=DIRECTION('ref_axis',(0.,-1.,0.));
#16661=DIRECTION('',(0.,-1.,0.));
#16662=DIRECTION('',(0.,-1.,0.));
#16663=DIRECTION('center_axis',(1.,0.,0.));
#16664=DIRECTION('ref_axis',(0.,0.,-1.));
#16665=DIRECTION('center_axis',(1.,0.,0.));
#16666=DIRECTION('ref_axis',(0.,0.,-1.));
#16667=DIRECTION('axis',(0.,0.,1.));
#16668=DIRECTION('refdir',(1.,0.,0.));
#16669=DIRECTION('center_axis',(0.,0.,1.));
#16670=DIRECTION('ref_axis',(1.,0.,0.));
#16671=DIRECTION('',(1.,0.,0.));
#16672=DIRECTION('',(0.,-1.,0.));
#16673=DIRECTION('',(-1.,0.,0.));
#16674=DIRECTION('',(0.,1.,0.));
#16675=DIRECTION('center_axis',(0.,1.,0.));
#16676=DIRECTION('ref_axis',(-1.,0.,0.));
#16677=DIRECTION('',(0.,0.,1.));
#16678=DIRECTION('',(-1.,0.,0.));
#16679=DIRECTION('',(0.,0.,1.));
#16680=DIRECTION('center_axis',(0.,0.,1.));
#16681=DIRECTION('ref_axis',(1.,0.,0.));
#16682=DIRECTION('',(0.,-1.,0.));
#16683=DIRECTION('',(1.,0.,0.));
#16684=DIRECTION('',(0.,1.,0.));
#16685=DIRECTION('center_axis',(0.,0.,-1.));
#16686=DIRECTION('ref_axis',(1.,0.,0.));
#16687=DIRECTION('center_axis',(-1.,0.,0.));
#16688=DIRECTION('ref_axis',(0.,-1.,0.));
#16689=DIRECTION('',(0.,0.,1.));
#16690=DIRECTION('',(0.,0.707106781186548,0.707106781186548));
#16691=DIRECTION('',(0.,-1.,0.));
#16692=DIRECTION('',(0.,0.707106781186548,-0.707106781186548));
#16693=DIRECTION('',(0.,0.,1.));
#16694=DIRECTION('',(0.,-1.,0.));
#16695=DIRECTION('',(0.,0.,1.));
#16696=DIRECTION('center_axis',(0.,-1.,0.));
#16697=DIRECTION('ref_axis',(1.,0.,0.));
#16698=DIRECTION('',(1.,0.,0.));
#16699=DIRECTION('',(0.,0.,1.));
#16700=DIRECTION('center_axis',(0.,0.,1.));
#16701=DIRECTION('ref_axis',(1.,0.,0.));
#16702=DIRECTION('',(-1.,0.,0.));
#16703=DIRECTION('',(0.,1.,0.));
#16704=DIRECTION('center_axis',(1.,0.,0.));
#16705=DIRECTION('ref_axis',(0.,1.,0.));
#16706=DIRECTION('',(0.,0.,1.));
#16707=DIRECTION('',(0.,-0.707106781186548,0.707106781186548));
#16708=DIRECTION('',(0.,1.,0.));
#16709=DIRECTION('',(0.,-0.707106781186548,-0.707106781186548));
#16710=DIRECTION('',(0.,0.,1.));
#16711=DIRECTION('center_axis',(0.,-1.,0.));
#16712=DIRECTION('ref_axis',(1.,0.,0.));
#16713=DIRECTION('',(-1.,0.,0.));
#16714=DIRECTION('center_axis',(0.,-0.707106781186548,-0.707106781186548));
#16715=DIRECTION('ref_axis',(-1.,0.,0.));
#16716=DIRECTION('',(1.,0.,0.));
#16717=DIRECTION('center_axis',(0.,0.707106781186548,0.707106781186548));
#16718=DIRECTION('ref_axis',(0.,0.707106781186547,-0.707106781186547));
#16719=DIRECTION('',(1.,0.,0.));
#16720=DIRECTION('center_axis',(0.,0.,1.));
#16721=DIRECTION('ref_axis',(1.,0.,0.));
#16722=DIRECTION('center_axis',(0.,0.,-1.));
#16723=DIRECTION('ref_axis',(1.,0.,0.));
#16724=DIRECTION('',(0.,0.,1.));
#16725=DIRECTION('center_axis',(0.,0.,-1.));
#16726=DIRECTION('ref_axis',(1.,0.,0.));
#16727=DIRECTION('center_axis',(0.,-0.707106781186548,0.707106781186548));
#16728=DIRECTION('ref_axis',(0.,0.707106781186547,0.707106781186547));
#16729=DIRECTION('center_axis',(0.,0.,-1.));
#16730=DIRECTION('ref_axis',(1.,0.,0.));
#16731=DIRECTION('center_axis',(0.,0.,1.));
#16732=DIRECTION('ref_axis',(1.,0.,0.));
#16733=DIRECTION('',(-1.,0.,0.));
#16734=DIRECTION('center_axis',(0.,0.,1.));
#16735=DIRECTION('ref_axis',(1.,0.,0.));
#16736=DIRECTION('',(-1.,0.,0.));
#16737=DIRECTION('center_axis',(0.,0.707106781186548,-0.707106781186548));
#16738=DIRECTION('ref_axis',(-1.,0.,0.));
#16739=DIRECTION('',(1.,0.,0.));
#16740=DIRECTION('center_axis',(0.,1.,0.));
#16741=DIRECTION('ref_axis',(-1.,0.,0.));
#16742=DIRECTION('axis',(0.,0.,1.));
#16743=DIRECTION('refdir',(1.,0.,0.));
#16744=DIRECTION('center_axis',(0.,1.,0.));
#16745=DIRECTION('ref_axis',(1.,0.,0.));
#16746=DIRECTION('center_axis',(0.,1.,0.));
#16747=DIRECTION('ref_axis',(1.,0.,0.));
#16748=DIRECTION('',(0.707106781186548,-0.707106781186547,-8.65956056235494E-17));
#16749=DIRECTION('center_axis',(0.,-1.,0.));
#16750=DIRECTION('ref_axis',(1.,0.,0.));
#16751=DIRECTION('center_axis',(0.,1.,0.));
#16752=DIRECTION('ref_axis',(1.,0.,0.));
#16753=DIRECTION('',(0.,-1.,0.));
#16754=DIRECTION('center_axis',(0.,-1.,0.));
#16755=DIRECTION('ref_axis',(1.,0.,0.));
#16756=DIRECTION('center_axis',(0.,1.,0.));
#16757=DIRECTION('ref_axis',(1.,0.,0.));
#16758=DIRECTION('center_axis',(0.,1.,0.));
#16759=DIRECTION('ref_axis',(1.,0.,0.));
#16760=DIRECTION('center_axis',(0.,1.,0.));
#16761=DIRECTION('ref_axis',(1.,0.,0.));
#16762=DIRECTION('',(0.,-1.,0.));
#16763=DIRECTION('center_axis',(0.,1.,0.));
#16764=DIRECTION('ref_axis',(1.,0.,0.));
#16765=DIRECTION('center_axis',(0.,1.,0.));
#16766=DIRECTION('ref_axis',(1.,0.,0.));
#16767=DIRECTION('axis',(0.,0.,1.));
#16768=DIRECTION('refdir',(1.,0.,0.));
#16769=DIRECTION('center_axis',(0.,0.,1.));
#16770=DIRECTION('ref_axis',(1.,0.,0.));
#16771=DIRECTION('center_axis',(0.,0.,1.));
#16772=DIRECTION('ref_axis',(1.,0.,0.));
#16773=DIRECTION('',(0.,0.,1.));
#16774=DIRECTION('center_axis',(0.,0.,-1.));
#16775=DIRECTION('ref_axis',(1.,0.,0.));
#16776=DIRECTION('center_axis',(0.,0.,1.));
#16777=DIRECTION('ref_axis',(1.,0.,0.));
#16778=DIRECTION('center_axis',(0.,0.,1.));
#16779=DIRECTION('ref_axis',(1.,0.,0.));
#16780=DIRECTION('center_axis',(0.,0.,1.));
#16781=DIRECTION('ref_axis',(1.,0.,0.));
#16782=DIRECTION('center_axis',(0.,0.,1.));
#16783=DIRECTION('ref_axis',(1.,0.,0.));
#16784=DIRECTION('',(0.,0.,1.));
#16785=DIRECTION('center_axis',(0.,0.,-1.));
#16786=DIRECTION('ref_axis',(1.,0.,0.));
#16787=DIRECTION('center_axis',(0.,0.,1.));
#16788=DIRECTION('ref_axis',(1.,0.,0.));
#16789=DIRECTION('center_axis',(0.,0.,1.));
#16790=DIRECTION('ref_axis',(1.,0.,0.));
#16791=DIRECTION('center_axis',(0.,0.,1.));
#16792=DIRECTION('ref_axis',(1.,0.,0.));
#16793=DIRECTION('center_axis',(0.,0.,1.));
#16794=DIRECTION('ref_axis',(1.,0.,0.));
#16795=DIRECTION('',(0.,0.,1.));
#16796=DIRECTION('center_axis',(0.,0.,-1.));
#16797=DIRECTION('ref_axis',(1.,0.,0.));
#16798=DIRECTION('center_axis',(0.,0.,1.));
#16799=DIRECTION('ref_axis',(1.,0.,0.));
#16800=DIRECTION('center_axis',(0.,0.,1.));
#16801=DIRECTION('ref_axis',(1.,0.,0.));
#16802=DIRECTION('center_axis',(0.,0.,1.));
#16803=DIRECTION('ref_axis',(1.,0.,0.));
#16804=DIRECTION('center_axis',(0.,0.,1.));
#16805=DIRECTION('ref_axis',(1.,0.,0.));
#16806=DIRECTION('',(0.,0.,1.));
#16807=DIRECTION('center_axis',(0.,0.,-1.));
#16808=DIRECTION('ref_axis',(1.,0.,0.));
#16809=DIRECTION('center_axis',(0.,0.,1.));
#16810=DIRECTION('ref_axis',(1.,0.,0.));
#16811=DIRECTION('center_axis',(0.,0.,1.));
#16812=DIRECTION('ref_axis',(1.,0.,0.));
#16813=DIRECTION('center_axis',(0.,0.,1.));
#16814=DIRECTION('ref_axis',(1.,0.,0.));
#16815=DIRECTION('center_axis',(0.,0.,1.));
#16816=DIRECTION('ref_axis',(1.,0.,0.));
#16817=DIRECTION('',(0.,0.,1.));
#16818=DIRECTION('center_axis',(0.,0.,1.));
#16819=DIRECTION('ref_axis',(1.,0.,0.));
#16820=DIRECTION('center_axis',(0.,0.,1.));
#16821=DIRECTION('ref_axis',(1.,0.,0.));
#16822=DIRECTION('',(0.,0.,1.));
#16823=DIRECTION('center_axis',(0.,0.,1.));
#16824=DIRECTION('ref_axis',(1.,0.,0.));
#16825=DIRECTION('center_axis',(0.,0.,1.));
#16826=DIRECTION('ref_axis',(1.,0.,0.));
#16827=DIRECTION('',(0.,0.,1.));
#16828=DIRECTION('center_axis',(0.,0.,1.));
#16829=DIRECTION('ref_axis',(1.,0.,0.));
#16830=DIRECTION('center_axis',(0.,0.,1.));
#16831=DIRECTION('ref_axis',(1.,0.,0.));
#16832=DIRECTION('',(0.,0.,1.));
#16833=DIRECTION('center_axis',(0.,-0.56333682464151,0.826227342807548));
#16834=DIRECTION('ref_axis',(0.,-0.826227342807548,-0.56333682464151));
#16835=DIRECTION('',(0.,-0.826227342807548,-0.56333682464151));
#16836=DIRECTION('',(1.,0.,0.));
#16837=DIRECTION('',(0.,-0.826227342807548,-0.56333682464151));
#16838=DIRECTION('',(1.,0.,0.));
#16839=DIRECTION('center_axis',(0.,-1.,0.));
#16840=DIRECTION('ref_axis',(0.,0.,-1.));
#16841=DIRECTION('',(0.,0.,-1.));
#16842=DIRECTION('',(0.,0.,-1.));
#16843=DIRECTION('',(1.,0.,0.));
#16844=DIRECTION('center_axis',(0.,-0.56333682464151,-0.826227342807548));
#16845=DIRECTION('ref_axis',(0.,0.826227342807548,-0.56333682464151));
#16846=DIRECTION('',(0.,0.826227342807548,-0.56333682464151));
#16847=DIRECTION('',(0.,0.826227342807548,-0.56333682464151));
#16848=DIRECTION('',(1.,0.,0.));
#16849=DIRECTION('center_axis',(0.,-1.,0.));
#16850=DIRECTION('ref_axis',(0.,0.,-1.));
#16851=DIRECTION('',(0.,0.,-1.));
#16852=DIRECTION('',(0.,0.,-1.));
#16853=DIRECTION('',(1.,0.,0.));
#16854=DIRECTION('center_axis',(0.,0.,1.));
#16855=DIRECTION('ref_axis',(0.,-1.,0.));
#16856=DIRECTION('',(0.,-1.,0.));
#16857=DIRECTION('',(0.,-1.,0.));
#16858=DIRECTION('',(1.,0.,0.));
#16859=DIRECTION('center_axis',(0.,1.,0.));
#16860=DIRECTION('ref_axis',(0.,0.,1.));
#16861=DIRECTION('',(0.,0.,1.));
#16862=DIRECTION('',(0.,0.,1.));
#16863=DIRECTION('',(1.,0.,0.));
#16864=DIRECTION('center_axis',(0.,0.56333682464151,-0.826227342807548));
#16865=DIRECTION('ref_axis',(0.,0.826227342807548,0.56333682464151));
#16866=DIRECTION('',(0.,0.826227342807548,0.56333682464151));
#16867=DIRECTION('',(0.,0.826227342807548,0.56333682464151));
#16868=DIRECTION('',(1.,0.,0.));
#16869=DIRECTION('center_axis',(0.,1.,0.));
#16870=DIRECTION('ref_axis',(0.,0.,1.));
#16871=DIRECTION('',(0.,0.,1.));
#16872=DIRECTION('',(0.,0.,1.));
#16873=DIRECTION('',(1.,0.,0.));
#16874=DIRECTION('center_axis',(0.,0.56333682464151,0.826227342807548));
#16875=DIRECTION('ref_axis',(0.,-0.826227342807548,0.56333682464151));
#16876=DIRECTION('',(0.,-0.826227342807548,0.56333682464151));
#16877=DIRECTION('',(0.,-0.826227342807548,0.56333682464151));
#16878=DIRECTION('',(1.,0.,0.));
#16879=DIRECTION('center_axis',(0.,1.,0.));
#16880=DIRECTION('ref_axis',(0.,0.,1.));
#16881=DIRECTION('',(0.,0.,1.));
#16882=DIRECTION('',(0.,0.,1.));
#16883=DIRECTION('',(1.,0.,0.));
#16884=DIRECTION('center_axis',(0.,0.,-1.));
#16885=DIRECTION('ref_axis',(0.,1.,0.));
#16886=DIRECTION('',(0.,1.,0.));
#16887=DIRECTION('',(0.,1.,0.));
#16888=DIRECTION('',(1.,0.,0.));
#16889=DIRECTION('center_axis',(0.,-1.,0.));
#16890=DIRECTION('ref_axis',(0.,0.,-1.));
#16891=DIRECTION('',(0.,0.,-1.));
#16892=DIRECTION('',(0.,0.,-1.));
#16893=DIRECTION('center_axis',(1.,0.,0.));
#16894=DIRECTION('ref_axis',(0.,0.,-1.));
#16895=DIRECTION('center_axis',(1.,0.,0.));
#16896=DIRECTION('ref_axis',(0.,0.,-1.));
#16897=DIRECTION('axis',(0.,0.,1.));
#16898=DIRECTION('refdir',(1.,0.,0.));
#16899=DIRECTION('center_axis',(0.,1.,0.));
#16900=DIRECTION('ref_axis',(0.,0.,1.));
#16901=DIRECTION('center_axis',(0.,-1.,0.));
#16902=DIRECTION('ref_axis',(1.,0.,0.));
#16903=DIRECTION('center_axis',(0.,-1.,0.));
#16904=DIRECTION('ref_axis',(1.,0.,0.));
#16905=DIRECTION('center_axis',(0.,-1.,0.));
#16906=DIRECTION('ref_axis',(1.,0.,0.));
#16907=DIRECTION('',(0.707106781186548,0.707106781186547,8.65956056235493E-17));
#16908=DIRECTION('center_axis',(0.,-1.,0.));
#16909=DIRECTION('ref_axis',(1.,0.,0.));
#16910=DIRECTION('center_axis',(0.,-1.,0.));
#16911=DIRECTION('ref_axis',(1.,0.,0.));
#16912=DIRECTION('',(0.,1.,0.));
#16913=DIRECTION('center_axis',(0.,1.,0.));
#16914=DIRECTION('ref_axis',(1.,0.,0.));
#16915=DIRECTION('center_axis',(0.,-1.,0.));
#16916=DIRECTION('ref_axis',(1.,0.,0.));
#16917=DIRECTION('',(-0.707106781186547,0.707106781186548,-8.65956056235493E-17));
#16918=DIRECTION('center_axis',(0.,-1.,0.));
#16919=DIRECTION('ref_axis',(0.,0.,-1.));
#16920=DIRECTION('center_axis',(0.,-1.,0.));
#16921=DIRECTION('ref_axis',(1.,0.,0.));
#16922=DIRECTION('center_axis',(0.,1.,0.));
#16923=DIRECTION('ref_axis',(1.,0.,0.));
#16924=DIRECTION('center_axis',(0.,1.,0.));
#16925=DIRECTION('ref_axis',(1.,0.,0.));
#16926=DIRECTION('',(-0.447213595499958,0.894427190999916,-5.47678698264203E-17));
#16927=DIRECTION('center_axis',(0.,-1.,0.));
#16928=DIRECTION('ref_axis',(1.,0.,0.));
#16929=DIRECTION('center_axis',(0.,1.,0.));
#16930=DIRECTION('ref_axis',(1.,0.,0.));
#16931=DIRECTION('',(0.,1.,0.));
#16932=DIRECTION('center_axis',(0.,1.,0.));
#16933=DIRECTION('ref_axis',(1.,0.,0.));
#16934=DIRECTION('center_axis',(0.,-1.,0.));
#16935=DIRECTION('ref_axis',(1.,0.,0.));
#16936=DIRECTION('',(-0.707106781186547,0.707106781186548,-8.65956056235493E-17));
#16937=DIRECTION('center_axis',(0.,-1.,0.));
#16938=DIRECTION('ref_axis',(0.,0.,-1.));
#16939=DIRECTION('center_axis',(0.866025403784439,0.,-0.5));
#16940=DIRECTION('ref_axis',(0.5,0.,0.866025403784439));
#16941=DIRECTION('',(-0.5,0.,-0.866025403784439));
#16942=DIRECTION('',(0.,-1.,0.));
#16943=DIRECTION('',(0.5,0.,0.866025403784439));
#16944=DIRECTION('',(0.,-1.,0.));
#16945=DIRECTION('center_axis',(1.20185167898973E-16,0.,-1.));
#16946=DIRECTION('ref_axis',(1.,0.,1.20185167898973E-16));
#16947=DIRECTION('',(-1.,0.,-1.20185167898973E-16));
#16948=DIRECTION('',(0.,-1.,0.));
#16949=DIRECTION('',(1.,0.,1.20185167898973E-16));
#16950=DIRECTION('center_axis',(-0.866025403784439,0.,-0.5));
#16951=DIRECTION('ref_axis',(0.5,0.,-0.866025403784439));
#16952=DIRECTION('',(-0.5,0.,0.866025403784439));
#16953=DIRECTION('',(0.,-1.,0.));
#16954=DIRECTION('',(0.5,0.,-0.866025403784439));
#16955=DIRECTION('center_axis',(-0.866025403784439,0.,0.5));
#16956=DIRECTION('ref_axis',(-0.5,0.,-0.866025403784439));
#16957=DIRECTION('',(0.5,0.,0.866025403784439));
#16958=DIRECTION('',(0.,-1.,0.));
#16959=DIRECTION('',(-0.5,0.,-0.866025403784439));
#16960=DIRECTION('center_axis',(-2.40370335797945E-16,0.,1.));
#16961=DIRECTION('ref_axis',(-1.,0.,-2.40370335797945E-16));
#16962=DIRECTION('',(1.,0.,2.40370335797945E-16));
#16963=DIRECTION('',(0.,-1.,0.));
#16964=DIRECTION('',(-1.,0.,-2.40370335797945E-16));
#16965=DIRECTION('center_axis',(0.866025403784439,0.,0.5));
#16966=DIRECTION('ref_axis',(-0.5,0.,0.866025403784439));
#16967=DIRECTION('',(0.5,0.,-0.866025403784439));
#16968=DIRECTION('',(-0.5,0.,0.866025403784439));
#16969=DIRECTION('center_axis',(0.,1.,0.));
#16970=DIRECTION('ref_axis',(1.,0.,0.));
#16971=DIRECTION('center_axis',(0.,-1.,0.));
#16972=DIRECTION('ref_axis',(0.,0.,-1.));
#16973=DIRECTION('axis',(0.,0.,1.));
#16974=DIRECTION('refdir',(1.,0.,0.));
#16975=DIRECTION('axis',(0.,0.,1.));
#16976=DIRECTION('refdir',(1.,0.,0.));
#16977=DIRECTION('center_axis',(0.,-1.,0.));
#16978=DIRECTION('ref_axis',(0.,0.,-1.));
#16979=DIRECTION('center_axis',(0.,-1.,0.));
#16980=DIRECTION('ref_axis',(1.,0.,0.));
#16981=DIRECTION('center_axis',(0.,-1.,0.));
#16982=DIRECTION('ref_axis',(1.,0.,0.));
#16983=DIRECTION('center_axis',(1.,0.,1.22464679914735E-16));
#16984=DIRECTION('ref_axis',(-1.22464679914735E-16,0.,1.));
#16985=DIRECTION('center_axis',(0.,1.,0.));
#16986=DIRECTION('ref_axis',(1.,0.,0.));
#16987=DIRECTION('center_axis',(0.,1.,0.));
#16988=DIRECTION('ref_axis',(1.,0.,0.));
#16989=DIRECTION('center_axis',(0.,-1.,0.));
#16990=DIRECTION('ref_axis',(1.,0.,0.));
#16991=DIRECTION('',(0.,1.,0.));
#16992=DIRECTION('center_axis',(0.,-1.,0.));
#16993=DIRECTION('ref_axis',(1.,0.,0.));
#16994=DIRECTION('center_axis',(0.,-1.,0.));
#16995=DIRECTION('ref_axis',(1.,0.,0.));
#16996=DIRECTION('center_axis',(0.,-1.,0.));
#16997=DIRECTION('ref_axis',(1.,0.,0.));
#16998=DIRECTION('',(0.,1.,0.));
#16999=DIRECTION('center_axis',(0.,-1.,0.));
#17000=DIRECTION('ref_axis',(1.,0.,0.));
#17001=DIRECTION('center_axis',(0.,1.,0.));
#17002=DIRECTION('ref_axis',(1.,0.,0.));
#17003=DIRECTION('',(-0.707106781186548,0.707106781186547,-8.65956056235493E-17));
#17004=DIRECTION('center_axis',(0.,-1.,0.));
#17005=DIRECTION('ref_axis',(1.,0.,0.));
#17006=DIRECTION('center_axis',(0.,1.,0.));
#17007=DIRECTION('ref_axis',(0.,0.,1.));
#17008=DIRECTION('center_axis',(0.,-1.,0.));
#17009=DIRECTION('ref_axis',(1.,0.,0.));
#17010=DIRECTION('center_axis',(0.,-1.,0.));
#17011=DIRECTION('ref_axis',(1.,0.,0.));
#17012=DIRECTION('',(0.,1.,0.));
#17013=DIRECTION('center_axis',(0.,-1.,0.));
#17014=DIRECTION('ref_axis',(0.,0.,-1.));
#17015=DIRECTION('center_axis',(0.,-1.,0.));
#17016=DIRECTION('ref_axis',(1.,0.,0.));
#17017=DIRECTION('center_axis',(0.,-1.,0.));
#17018=DIRECTION('ref_axis',(1.,0.,0.));
#17019=DIRECTION('',(0.707106781186548,0.707106781186547,8.65956056235493E-17));
#17020=DIRECTION('axis',(0.,0.,1.));
#17021=DIRECTION('refdir',(1.,0.,0.));
#17022=DIRECTION('center_axis',(0.,-1.,0.));
#17023=DIRECTION('ref_axis',(0.,0.,-1.));
#17024=DIRECTION('center_axis',(0.,-1.,0.));
#17025=DIRECTION('ref_axis',(1.,0.,0.));
#17026=DIRECTION('center_axis',(0.,-1.,0.));
#17027=DIRECTION('ref_axis',(1.,0.,0.));
#17028=DIRECTION('center_axis',(1.,0.,1.22464679914735E-16));
#17029=DIRECTION('ref_axis',(-1.22464679914735E-16,0.,1.));
#17030=DIRECTION('center_axis',(0.,1.,0.));
#17031=DIRECTION('ref_axis',(1.,0.,0.));
#17032=DIRECTION('center_axis',(0.,1.,0.));
#17033=DIRECTION('ref_axis',(1.,0.,0.));
#17034=DIRECTION('center_axis',(0.,-1.,0.));
#17035=DIRECTION('ref_axis',(1.,0.,0.));
#17036=DIRECTION('center_axis',(0.,-1.,0.));
#17037=DIRECTION('ref_axis',(1.,0.,0.));
#17038=DIRECTION('',(0.,1.,0.));
#17039=DIRECTION('center_axis',(0.,1.,0.));
#17040=DIRECTION('ref_axis',(0.,0.,1.));
#17041=DIRECTION('center_axis',(0.,-1.,0.));
#17042=DIRECTION('ref_axis',(1.,0.,0.));
#17043=DIRECTION('center_axis',(0.,-1.,0.));
#17044=DIRECTION('ref_axis',(1.,0.,0.));
#17045=DIRECTION('center_axis',(0.,-1.,0.));
#17046=DIRECTION('ref_axis',(1.,0.,0.));
#17047=DIRECTION('center_axis',(0.,-1.,0.));
#17048=DIRECTION('ref_axis',(1.,0.,0.));
#17049=DIRECTION('',(0.707106781186548,0.707106781186547,8.65956056235494E-17));
#17050=DIRECTION('center_axis',(0.,-1.,0.));
#17051=DIRECTION('ref_axis',(1.,0.,0.));
#17052=DIRECTION('center_axis',(0.,-1.,0.));
#17053=DIRECTION('ref_axis',(1.,0.,0.));
#17054=DIRECTION('',(0.,1.,0.));
#17055=DIRECTION('center_axis',(0.,1.,0.));
#17056=DIRECTION('ref_axis',(1.,0.,0.));
#17057=DIRECTION('center_axis',(0.,-1.,0.));
#17058=DIRECTION('ref_axis',(1.,0.,0.));
#17059=DIRECTION('',(-0.707106781186548,0.707106781186547,-8.65956056235494E-17));
#17060=DIRECTION('center_axis',(0.,-1.,0.));
#17061=DIRECTION('ref_axis',(0.,0.,-1.));
#17062=DIRECTION('center_axis',(0.,-1.,0.));
#17063=DIRECTION('ref_axis',(1.,0.,0.));
#17064=DIRECTION('',(0.,1.,0.));
#17065=DIRECTION('axis',(0.,0.,1.));
#17066=DIRECTION('refdir',(1.,0.,0.));
#17067=DIRECTION('center_axis',(0.,0.,1.));
#17068=DIRECTION('ref_axis',(1.,0.,0.));
#17069=DIRECTION('center_axis',(1.22464679914735E-16,-1.,0.));
#17070=DIRECTION('ref_axis',(-1.,-1.22464679914735E-16,0.));
#17071=DIRECTION('center_axis',(0.78183148246803,0.,0.623489801858733));
#17072=DIRECTION('ref_axis',(0.623489801858734,0.,-0.78183148246803));
#17073=DIRECTION('center_axis',(7.63554790147315E-17,-1.,-9.57467422477103E-17));
#17074=DIRECTION('ref_axis',(-0.623489801858734,-1.22464679914735E-16,0.78183148246803));
#17075=DIRECTION('center_axis',(0.974927912181824,0.,-0.222520933956314));
#17076=DIRECTION('ref_axis',(-0.222520933956314,0.,-0.974927912181824));
#17077=DIRECTION('center_axis',(-2.7250954951288E-17,-1.,-1.19394234705288E-16));
#17078=DIRECTION('ref_axis',(0.222520933956314,-1.22464679914735E-16,0.974927912181824));
#17079=DIRECTION('center_axis',(0.433883739117558,0.,-0.900968867902419));
#17080=DIRECTION('ref_axis',(-0.900968867902419,0.,-0.433883739117558));
#17081=DIRECTION('center_axis',(-1.10336864020811E-16,-1.,-5.31354332312403E-17));
#17082=DIRECTION('ref_axis',(0.900968867902419,-1.22464679914735E-16,0.433883739117558));
#17083=DIRECTION('center_axis',(-0.433883739117558,0.,-0.900968867902419));
#17084=DIRECTION('ref_axis',(-0.900968867902419,0.,0.433883739117558));
#17085=DIRECTION('center_axis',(-1.10336864020811E-16,-1.,5.31354332312403E-17));
#17086=DIRECTION('ref_axis',(0.900968867902419,-1.22464679914735E-16,-0.433883739117558));
#17087=DIRECTION('center_axis',(-0.974927912181824,0.,-0.222520933956314));
#17088=DIRECTION('ref_axis',(-0.222520933956315,0.,0.974927912181824));
#17089=DIRECTION('center_axis',(-2.7250954951288E-17,-1.,1.19394234705288E-16));
#17090=DIRECTION('ref_axis',(0.222520933956315,-1.22464679914735E-16,-0.974927912181824));
#17091=DIRECTION('center_axis',(-0.78183148246803,0.,0.623489801858734));
#17092=DIRECTION('ref_axis',(0.623489801858733,0.,0.78183148246803));
#17093=DIRECTION('center_axis',(7.63554790147315E-17,-1.,9.57467422477103E-17));
#17094=DIRECTION('ref_axis',(-0.623489801858733,-1.22464679914735E-16,-0.78183148246803));
#17095=DIRECTION('axis',(0.,0.,1.));
#17096=DIRECTION('refdir',(1.,0.,0.));
#17097=DIRECTION('center_axis',(0.,0.,1.));
#17098=DIRECTION('ref_axis',(1.,0.,0.));
#17099=DIRECTION('center_axis',(0.,-1.,0.));
#17100=DIRECTION('ref_axis',(0.,0.,-1.));
#17101=DIRECTION('center_axis',(0.,-1.,0.));
#17102=DIRECTION('ref_axis',(0.,0.,-1.));
#17103=DIRECTION('center_axis',(0.,1.,0.));
#17104=DIRECTION('ref_axis',(1.,0.,0.));
#17105=DIRECTION('center_axis',(0.,1.,0.));
#17106=DIRECTION('ref_axis',(1.,0.,0.));
#17107=DIRECTION('center_axis',(0.,1.,0.));
#17108=DIRECTION('ref_axis',(1.,0.,0.));
#17109=DIRECTION('center_axis',(0.,1.,0.));
#17110=DIRECTION('ref_axis',(1.,0.,0.));
#17111=DIRECTION('',(0.,-1.,0.));
#17112=DIRECTION('center_axis',(0.,-1.,0.));
#17113=DIRECTION('ref_axis',(1.,0.,0.));
#17114=DIRECTION('center_axis',(0.,1.,0.));
#17115=DIRECTION('ref_axis',(1.,0.,0.));
#17116=DIRECTION('center_axis',(0.,1.,0.));
#17117=DIRECTION('ref_axis',(1.,0.,0.));
#17118=DIRECTION('center_axis',(0.,1.,0.));
#17119=DIRECTION('ref_axis',(1.,0.,0.));
#17120=DIRECTION('center_axis',(0.,1.,0.));
#17121=DIRECTION('ref_axis',(1.,0.,0.));
#17122=DIRECTION('center_axis',(0.,1.,0.));
#17123=DIRECTION('ref_axis',(1.,0.,0.));
#17124=DIRECTION('center_axis',(0.,1.,0.));
#17125=DIRECTION('ref_axis',(1.,0.,0.));
#17126=DIRECTION('center_axis',(0.,-1.,0.));
#17127=DIRECTION('ref_axis',(1.,0.,0.));
#17128=DIRECTION('center_axis',(0.,-1.,0.));
#17129=DIRECTION('ref_axis',(0.,0.,-1.));
#17130=DIRECTION('center_axis',(8.96625347776458E-17,0.,1.));
#17131=DIRECTION('ref_axis',(1.,0.,0.));
#17132=DIRECTION('center_axis',(0.,-1.,0.));
#17133=DIRECTION('ref_axis',(0.,0.,-1.));
#17134=DIRECTION('center_axis',(0.,1.,0.));
#17135=DIRECTION('ref_axis',(1.,0.,0.));
#17136=DIRECTION('center_axis',(0.,-1.,0.));
#17137=DIRECTION('ref_axis',(1.,0.,0.));
#17138=DIRECTION('center_axis',(0.,-1.,0.));
#17139=DIRECTION('ref_axis',(0.,0.,-1.));
#17140=DIRECTION('center_axis',(0.,0.,1.));
#17141=DIRECTION('ref_axis',(1.,0.,0.));
#17142=DIRECTION('center_axis',(0.,-1.,0.));
#17143=DIRECTION('ref_axis',(0.,0.,-1.));
#17144=DIRECTION('center_axis',(0.,1.,0.));
#17145=DIRECTION('ref_axis',(1.,0.,0.));
#17146=DIRECTION('center_axis',(0.,-1.,0.));
#17147=DIRECTION('ref_axis',(1.,0.,0.));
#17148=DIRECTION('center_axis',(0.,-1.,0.));
#17149=DIRECTION('ref_axis',(1.,0.,0.));
#17150=DIRECTION('center_axis',(0.,-1.,0.));
#17151=DIRECTION('ref_axis',(0.,0.,-1.));
#17152=DIRECTION('center_axis',(0.,0.,1.));
#17153=DIRECTION('ref_axis',(1.,0.,0.));
#17154=DIRECTION('center_axis',(0.,-1.,0.));
#17155=DIRECTION('ref_axis',(0.,0.,-1.));
#17156=DIRECTION('center_axis',(0.,1.,0.));
#17157=DIRECTION('ref_axis',(1.,0.,0.));
#17158=DIRECTION('center_axis',(0.,-1.,0.));
#17159=DIRECTION('ref_axis',(1.,0.,0.));
#17160=DIRECTION('center_axis',(0.,-1.,0.));
#17161=DIRECTION('ref_axis',(0.,0.,-1.));
#17162=DIRECTION('center_axis',(8.96625347776458E-17,0.,1.));
#17163=DIRECTION('ref_axis',(1.,0.,0.));
#17164=DIRECTION('center_axis',(0.,-1.,0.));
#17165=DIRECTION('ref_axis',(0.,0.,-1.));
#17166=DIRECTION('center_axis',(0.,1.,0.));
#17167=DIRECTION('ref_axis',(1.,0.,0.));
#17168=DIRECTION('center_axis',(0.,-1.,0.));
#17169=DIRECTION('ref_axis',(1.,0.,0.));
#17170=DIRECTION('center_axis',(0.,-1.,0.));
#17171=DIRECTION('ref_axis',(0.,0.,-1.));
#17172=DIRECTION('center_axis',(0.,0.,1.));
#17173=DIRECTION('ref_axis',(1.,0.,0.));
#17174=DIRECTION('center_axis',(0.,-1.,0.));
#17175=DIRECTION('ref_axis',(0.,0.,-1.));
#17176=DIRECTION('center_axis',(0.,1.,0.));
#17177=DIRECTION('ref_axis',(1.,0.,0.));
#17178=DIRECTION('center_axis',(0.,1.,0.));
#17179=DIRECTION('ref_axis',(1.,0.,0.));
#17180=DIRECTION('',(0.,1.,0.));
#17181=DIRECTION('center_axis',(0.,-1.,0.));
#17182=DIRECTION('ref_axis',(1.,0.,0.));
#17183=DIRECTION('center_axis',(0.,-1.,0.));
#17184=DIRECTION('ref_axis',(1.,0.,0.));
#17185=DIRECTION('center_axis',(0.,1.,0.));
#17186=DIRECTION('ref_axis',(1.,0.,0.));
#17187=DIRECTION('center_axis',(0.,-1.,0.));
#17188=DIRECTION('ref_axis',(0.,0.,-1.));
#17189=DIRECTION('center_axis',(0.,0.,1.));
#17190=DIRECTION('ref_axis',(1.,0.,0.));
#17191=DIRECTION('center_axis',(0.,-1.,0.));
#17192=DIRECTION('ref_axis',(0.,0.,-1.));
#17193=DIRECTION('center_axis',(0.,-1.,0.));
#17194=DIRECTION('ref_axis',(-1.,0.,0.));
#17195=DIRECTION('center_axis',(0.,1.,0.));
#17196=DIRECTION('ref_axis',(1.,0.,0.));
#17197=DIRECTION('axis',(0.,0.,1.));
#17198=DIRECTION('refdir',(1.,0.,0.));
#17199=DIRECTION('center_axis',(0.,1.,0.));
#17200=DIRECTION('ref_axis',(0.,0.,1.));
#17201=DIRECTION('center_axis',(0.,-1.,0.));
#17202=DIRECTION('ref_axis',(1.,0.,0.));
#17203=DIRECTION('center_axis',(0.,-1.,0.));
#17204=DIRECTION('ref_axis',(1.,0.,0.));
#17205=DIRECTION('center_axis',(0.,-1.,0.));
#17206=DIRECTION('ref_axis',(1.,0.,0.));
#17207=DIRECTION('center_axis',(0.,-1.,0.));
#17208=DIRECTION('ref_axis',(1.,0.,0.));
#17209=DIRECTION('',(0.,1.,0.));
#17210=DIRECTION('center_axis',(0.,-1.,0.));
#17211=DIRECTION('ref_axis',(0.,0.,-1.));
#17212=DIRECTION('center_axis',(0.,-1.,0.));
#17213=DIRECTION('ref_axis',(1.,0.,0.));
#17214=DIRECTION('center_axis',(0.,-1.,0.));
#17215=DIRECTION('ref_axis',(1.,0.,0.));
#17216=DIRECTION('',(0.,1.,0.));
#17217=DIRECTION('center_axis',(0.,1.,0.));
#17218=DIRECTION('ref_axis',(0.,0.,1.));
#17219=DIRECTION('center_axis',(0.,-1.,0.));
#17220=DIRECTION('ref_axis',(1.,0.,0.));
#17221=DIRECTION('center_axis',(0.,-1.,0.));
#17222=DIRECTION('ref_axis',(1.,0.,0.));
#17223=DIRECTION('center_axis',(0.,-1.,0.));
#17224=DIRECTION('ref_axis',(1.,0.,0.));
#17225=DIRECTION('center_axis',(0.,-1.,0.));
#17226=DIRECTION('ref_axis',(1.,0.,0.));
#17227=DIRECTION('',(0.,1.,0.));
#17228=DIRECTION('center_axis',(0.,-1.,0.));
#17229=DIRECTION('ref_axis',(0.,0.,-1.));
#17230=DIRECTION('center_axis',(0.,-1.,0.));
#17231=DIRECTION('ref_axis',(1.,0.,0.));
#17232=DIRECTION('center_axis',(0.,-1.,0.));
#17233=DIRECTION('ref_axis',(1.,0.,0.));
#17234=DIRECTION('',(0.,1.,0.));
#17235=DIRECTION('',(0.,0.,1.));
#17236=DIRECTION('',(1.,0.,0.));
#17237=DIRECTION('',(0.,0.,1.));
#17238=DIRECTION('',(1.,0.,0.));
#17239=DIRECTION('',(0.,0.,1.));
#17240=DIRECTION('',(1.,0.,0.));
#17241=DIRECTION('',(0.,0.,1.));
#17242=DIRECTION('',(1.,0.,0.));
#17243=DIRECTION('',(0.,0.,1.));
#17244=DIRECTION('',(1.,0.,0.));
#17245=DIRECTION('axis',(0.,0.,1.));
#17246=DIRECTION('refdir',(1.,0.,0.));
#17247=DIRECTION('center_axis',(0.866025403784439,0.,-0.5));
#17248=DIRECTION('ref_axis',(0.5,0.,0.866025403784439));
#17249=DIRECTION('',(-0.5,0.,-0.866025403784439));
#17250=DIRECTION('',(0.,-1.,0.));
#17251=DIRECTION('',(0.5,0.,0.866025403784439));
#17252=DIRECTION('',(0.,-1.,0.));
#17253=DIRECTION('center_axis',(1.60246890531964E-16,0.,-1.));
#17254=DIRECTION('ref_axis',(1.,0.,1.60246890531964E-16));
#17255=DIRECTION('',(-1.,0.,-1.60246890531964E-16));
#17256=DIRECTION('',(0.,-1.,0.));
#17257=DIRECTION('',(1.,0.,1.60246890531964E-16));
#17258=DIRECTION('center_axis',(-0.866025403784439,0.,-0.5));
#17259=DIRECTION('ref_axis',(0.5,0.,-0.866025403784439));
#17260=DIRECTION('',(-0.5,0.,0.866025403784439));
#17261=DIRECTION('',(0.,-1.,0.));
#17262=DIRECTION('',(0.5,0.,-0.866025403784439));
#17263=DIRECTION('center_axis',(-0.866025403784439,0.,0.5));
#17264=DIRECTION('ref_axis',(-0.5,0.,-0.866025403784439));
#17265=DIRECTION('',(0.5,0.,0.866025403784439));
#17266=DIRECTION('',(0.,-1.,0.));
#17267=DIRECTION('',(-0.5,0.,-0.866025403784439));
#17268=DIRECTION('center_axis',(-1.60246890531964E-16,0.,1.));
#17269=DIRECTION('ref_axis',(-1.,0.,-1.60246890531964E-16));
#17270=DIRECTION('',(1.,0.,1.60246890531964E-16));
#17271=DIRECTION('',(0.,-1.,0.));
#17272=DIRECTION('',(-1.,0.,-1.60246890531964E-16));
#17273=DIRECTION('center_axis',(0.866025403784439,0.,0.5));
#17274=DIRECTION('ref_axis',(-0.5,0.,0.866025403784439));
#17275=DIRECTION('',(0.5,0.,-0.866025403784439));
#17276=DIRECTION('',(-0.5,0.,0.866025403784439));
#17277=DIRECTION('center_axis',(0.,1.,0.));
#17278=DIRECTION('ref_axis',(1.,0.,0.));
#17279=DIRECTION('center_axis',(0.,-1.,0.));
#17280=DIRECTION('ref_axis',(0.,0.,-1.));
#17281=DIRECTION('center_axis',(0.,1.,0.));
#17282=DIRECTION('ref_axis',(1.,0.,0.));
#17283=DIRECTION('center_axis',(0.,1.,0.));
#17284=DIRECTION('ref_axis',(1.,0.,0.));
#17285=DIRECTION('center_axis',(0.,1.,0.));
#17286=DIRECTION('ref_axis',(0.,0.,1.));
#17287=DIRECTION('center_axis',(0.,-1.,0.));
#17288=DIRECTION('ref_axis',(1.,0.,0.));
#17289=DIRECTION('center_axis',(0.,-1.,0.));
#17290=DIRECTION('ref_axis',(1.,0.,0.));
#17291=DIRECTION('center_axis',(0.,-1.,0.));
#17292=DIRECTION('ref_axis',(1.,0.,0.));
#17293=DIRECTION('',(0.707106781186547,0.707106781186548,8.65956056235493E-17));
#17294=DIRECTION('center_axis',(0.,-1.,0.));
#17295=DIRECTION('ref_axis',(1.,0.,0.));
#17296=DIRECTION('center_axis',(0.,-1.,0.));
#17297=DIRECTION('ref_axis',(1.,0.,0.));
#17298=DIRECTION('',(0.,1.,0.));
#17299=DIRECTION('center_axis',(0.,1.,0.));
#17300=DIRECTION('ref_axis',(1.,0.,0.));
#17301=DIRECTION('center_axis',(0.,-1.,0.));
#17302=DIRECTION('ref_axis',(1.,0.,0.));
#17303=DIRECTION('',(-0.707106781186547,0.707106781186548,-8.65956056235493E-17));
#17304=DIRECTION('center_axis',(0.,-1.,0.));
#17305=DIRECTION('ref_axis',(0.,0.,-1.));
#17306=DIRECTION('center_axis',(0.,-1.,0.));
#17307=DIRECTION('ref_axis',(1.,0.,0.));
#17308=DIRECTION('center_axis',(0.,1.,0.));
#17309=DIRECTION('ref_axis',(1.,0.,0.));
#17310=DIRECTION('center_axis',(0.,1.,0.));
#17311=DIRECTION('ref_axis',(1.,0.,0.));
#17312=DIRECTION('',(-0.447213595499958,0.894427190999916,-5.47678698264203E-17));
#17313=DIRECTION('center_axis',(0.,-1.,0.));
#17314=DIRECTION('ref_axis',(1.,0.,0.));
#17315=DIRECTION('',(0.,1.,0.));
#17316=DIRECTION('axis',(0.,0.,1.));
#17317=DIRECTION('refdir',(1.,0.,0.));
#17318=DIRECTION('axis',(0.,0.,1.));
#17319=DIRECTION('refdir',(1.,0.,0.));
#17320=DIRECTION('center_axis',(0.,0.,1.));
#17321=DIRECTION('ref_axis',(1.,0.,0.));
#17322=DIRECTION('center_axis',(0.,0.,1.));
#17323=DIRECTION('ref_axis',(1.,0.,0.));
#17324=DIRECTION('',(0.,0.,1.));
#17325=DIRECTION('center_axis',(0.,0.,-1.));
#17326=DIRECTION('ref_axis',(1.,0.,0.));
#17327=DIRECTION('center_axis',(0.,0.,1.));
#17328=DIRECTION('ref_axis',(1.,0.,0.));
#17329=DIRECTION('center_axis',(0.,0.,1.));
#17330=DIRECTION('ref_axis',(1.,0.,0.));
#17331=DIRECTION('',(0.,0.,1.));
#17332=DIRECTION('center_axis',(0.,0.,-1.));
#17333=DIRECTION('ref_axis',(1.,0.,0.));
#17334=DIRECTION('center_axis',(0.,0.,1.));
#17335=DIRECTION('ref_axis',(1.,0.,0.));
#17336=DIRECTION('center_axis',(0.,0.,1.));
#17337=DIRECTION('ref_axis',(1.,0.,0.));
#17338=DIRECTION('',(0.,0.,1.));
#17339=DIRECTION('center_axis',(0.,0.,-1.));
#17340=DIRECTION('ref_axis',(1.,0.,0.));
#17341=DIRECTION('center_axis',(0.,0.,1.));
#17342=DIRECTION('ref_axis',(1.,0.,0.));
#17343=DIRECTION('center_axis',(0.,0.,1.));
#17344=DIRECTION('ref_axis',(1.,0.,0.));
#17345=DIRECTION('',(0.,0.,1.));
#17346=DIRECTION('center_axis',(0.,0.,-1.));
#17347=DIRECTION('ref_axis',(1.,0.,0.));
#17348=DIRECTION('center_axis',(0.,0.,1.));
#17349=DIRECTION('ref_axis',(1.,0.,0.));
#17350=DIRECTION('center_axis',(0.,0.,1.));
#17351=DIRECTION('ref_axis',(1.,0.,0.));
#17352=DIRECTION('',(0.,0.,1.));
#17353=DIRECTION('center_axis',(0.,0.,-1.));
#17354=DIRECTION('ref_axis',(1.,0.,0.));
#17355=DIRECTION('center_axis',(0.,0.,1.));
#17356=DIRECTION('ref_axis',(1.,0.,0.));
#17357=DIRECTION('center_axis',(0.,0.,1.));
#17358=DIRECTION('ref_axis',(1.,0.,0.));
#17359=DIRECTION('',(0.,0.,1.));
#17360=DIRECTION('center_axis',(0.,0.,-1.));
#17361=DIRECTION('ref_axis',(1.,0.,0.));
#17362=DIRECTION('center_axis',(0.,0.,1.));
#17363=DIRECTION('ref_axis',(1.,0.,0.));
#17364=DIRECTION('center_axis',(0.,0.,1.));
#17365=DIRECTION('ref_axis',(1.,0.,0.));
#17366=DIRECTION('',(0.,0.,1.));
#17367=DIRECTION('center_axis',(0.,0.,-1.));
#17368=DIRECTION('ref_axis',(1.,0.,0.));
#17369=DIRECTION('center_axis',(0.,0.,1.));
#17370=DIRECTION('ref_axis',(1.,0.,0.));
#17371=DIRECTION('center_axis',(0.,0.,1.));
#17372=DIRECTION('ref_axis',(1.,0.,0.));
#17373=DIRECTION('',(0.,0.,1.));
#17374=DIRECTION('center_axis',(0.,0.,-1.));
#17375=DIRECTION('ref_axis',(1.,0.,0.));
#17376=DIRECTION('center_axis',(0.,1.,0.));
#17377=DIRECTION('ref_axis',(-1.,0.,0.));
#17378=DIRECTION('',(-1.,0.,0.));
#17379=DIRECTION('',(0.,0.,1.));
#17380=DIRECTION('',(-1.,0.,0.));
#17381=DIRECTION('',(0.,0.,1.));
#17382=DIRECTION('center_axis',(1.,0.,0.));
#17383=DIRECTION('ref_axis',(0.,1.,0.));
#17384=DIRECTION('',(0.,1.,0.));
#17385=DIRECTION('',(0.,1.,0.));
#17386=DIRECTION('',(0.,0.,1.));
#17387=DIRECTION('center_axis',(0.,-1.,0.));
#17388=DIRECTION('ref_axis',(1.,0.,0.));
#17389=DIRECTION('',(1.,0.,0.));
#17390=DIRECTION('',(1.,0.,0.));
#17391=DIRECTION('',(0.,0.,1.));
#17392=DIRECTION('center_axis',(-1.,0.,0.));
#17393=DIRECTION('ref_axis',(0.,-1.,0.));
#17394=DIRECTION('',(0.,-1.,0.));
#17395=DIRECTION('',(0.,-1.,0.));
#17396=DIRECTION('center_axis',(0.,0.,1.));
#17397=DIRECTION('ref_axis',(1.,0.,0.));
#17398=DIRECTION('center_axis',(0.,0.,1.));
#17399=DIRECTION('ref_axis',(1.,0.,0.));
#17400=DIRECTION('axis',(0.,0.,1.));
#17401=DIRECTION('refdir',(1.,0.,0.));
#17402=DIRECTION('center_axis',(0.,0.,1.));
#17403=DIRECTION('ref_axis',(1.,0.,0.));
#17404=DIRECTION('center_axis',(0.,0.,1.));
#17405=DIRECTION('ref_axis',(1.,0.,0.));
#17406=DIRECTION('',(0.,0.,1.));
#17407=DIRECTION('center_axis',(0.,0.,1.));
#17408=DIRECTION('ref_axis',(1.,0.,0.));
#17409=DIRECTION('center_axis',(0.,0.,1.));
#17410=DIRECTION('ref_axis',(1.,0.,0.));
#17411=DIRECTION('center_axis',(0.,0.,1.));
#17412=DIRECTION('ref_axis',(1.,0.,0.));
#17413=DIRECTION('center_axis',(0.,0.,1.));
#17414=DIRECTION('ref_axis',(1.,0.,0.));
#17415=DIRECTION('',(0.,0.,1.));
#17416=DIRECTION('center_axis',(0.,0.,1.));
#17417=DIRECTION('ref_axis',(1.,0.,0.));
#17418=DIRECTION('center_axis',(0.,0.,1.));
#17419=DIRECTION('ref_axis',(1.,0.,0.));
#17420=DIRECTION('center_axis',(0.,0.,1.));
#17421=DIRECTION('ref_axis',(1.,0.,0.));
#17422=DIRECTION('center_axis',(0.,0.,1.));
#17423=DIRECTION('ref_axis',(1.,0.,0.));
#17424=DIRECTION('',(0.,0.,1.));
#17425=DIRECTION('center_axis',(0.,0.,1.));
#17426=DIRECTION('ref_axis',(1.,0.,0.));
#17427=DIRECTION('center_axis',(0.,0.,1.));
#17428=DIRECTION('ref_axis',(1.,0.,0.));
#17429=DIRECTION('center_axis',(0.,0.,1.));
#17430=DIRECTION('ref_axis',(1.,0.,0.));
#17431=DIRECTION('center_axis',(0.,0.,1.));
#17432=DIRECTION('ref_axis',(1.,0.,0.));
#17433=DIRECTION('',(0.,0.,1.));
#17434=DIRECTION('center_axis',(0.,0.,1.));
#17435=DIRECTION('ref_axis',(1.,0.,0.));
#17436=DIRECTION('center_axis',(0.,0.,1.));
#17437=DIRECTION('ref_axis',(1.,0.,0.));
#17438=DIRECTION('center_axis',(-1.,0.,0.));
#17439=DIRECTION('ref_axis',(0.,0.,1.));
#17440=DIRECTION('',(0.,0.,-1.));
#17441=DIRECTION('',(0.,1.,0.));
#17442=DIRECTION('',(0.,0.,1.));
#17443=DIRECTION('',(0.,1.,0.));
#17444=DIRECTION('center_axis',(0.,0.,-1.));
#17445=DIRECTION('ref_axis',(-1.,0.,0.));
#17446=DIRECTION('',(1.,0.,0.));
#17447=DIRECTION('',(-1.,0.,0.));
#17448=DIRECTION('',(0.,1.,0.));
#17449=DIRECTION('center_axis',(1.,0.,0.));
#17450=DIRECTION('ref_axis',(0.,0.,-1.));
#17451=DIRECTION('',(0.,0.,1.));
#17452=DIRECTION('',(0.,0.,-1.));
#17453=DIRECTION('',(0.,1.,0.));
#17454=DIRECTION('center_axis',(0.,0.,1.));
#17455=DIRECTION('ref_axis',(1.,0.,0.));
#17456=DIRECTION('',(-1.,0.,0.));
#17457=DIRECTION('',(1.,0.,0.));
#17458=DIRECTION('',(0.,1.,0.));
#17459=DIRECTION('center_axis',(0.939692620785911,0.,0.342020143325662));
#17460=DIRECTION('ref_axis',(0.342020143325662,0.,-0.939692620785911));
#17461=DIRECTION('',(-0.342020143325662,0.,0.939692620785911));
#17462=DIRECTION('',(0.342020143325662,0.,-0.939692620785911));
#17463=DIRECTION('',(0.,1.,0.));
#17464=DIRECTION('center_axis',(0.,0.,1.));
#17465=DIRECTION('ref_axis',(1.,0.,0.));
#17466=DIRECTION('',(-1.,0.,0.));
#17467=DIRECTION('',(1.,0.,0.));
#17468=DIRECTION('',(0.,1.,0.));
#17469=DIRECTION('center_axis',(-0.939692620785908,0.,0.342020143325669));
#17470=DIRECTION('ref_axis',(0.342020143325669,0.,0.939692620785908));
#17471=DIRECTION('',(-0.342020143325669,0.,-0.939692620785908));
#17472=DIRECTION('',(0.342020143325669,0.,0.939692620785908));
#17473=DIRECTION('',(0.,1.,0.));
#17474=DIRECTION('center_axis',(0.,0.,1.));
#17475=DIRECTION('ref_axis',(1.,0.,0.));
#17476=DIRECTION('',(-1.,0.,0.));
#17477=DIRECTION('',(1.,0.,0.));
#17478=DIRECTION('',(0.,1.,0.));
#17479=DIRECTION('center_axis',(0.939692620785908,0.,0.342020143325669));
#17480=DIRECTION('ref_axis',(0.342020143325669,0.,-0.939692620785908));
#17481=DIRECTION('',(-0.342020143325669,0.,0.939692620785908));
#17482=DIRECTION('',(0.342020143325669,0.,-0.939692620785908));
#17483=DIRECTION('',(0.,1.,0.));
#17484=DIRECTION('center_axis',(0.,0.,1.));
#17485=DIRECTION('ref_axis',(1.,0.,0.));
#17486=DIRECTION('',(-1.,0.,0.));
#17487=DIRECTION('',(1.,0.,0.));
#17488=DIRECTION('',(0.,1.,0.));
#17489=DIRECTION('center_axis',(-0.939692620785908,0.,0.342020143325669));
#17490=DIRECTION('ref_axis',(0.342020143325669,0.,0.939692620785908));
#17491=DIRECTION('',(-0.342020143325669,0.,-0.939692620785908));
#17492=DIRECTION('',(0.342020143325669,0.,0.939692620785908));
#17493=DIRECTION('',(0.,1.,0.));
#17494=DIRECTION('center_axis',(0.,0.,1.));
#17495=DIRECTION('ref_axis',(1.,0.,0.));
#17496=DIRECTION('',(-1.,0.,0.));
#17497=DIRECTION('',(1.,0.,0.));
#17498=DIRECTION('',(0.,1.,0.));
#17499=DIRECTION('center_axis',(0.939692620785908,0.,0.342020143325669));
#17500=DIRECTION('ref_axis',(0.342020143325669,0.,-0.939692620785908));
#17501=DIRECTION('',(-0.342020143325669,0.,0.939692620785908));
#17502=DIRECTION('',(0.342020143325669,0.,-0.939692620785908));
#17503=DIRECTION('',(0.,1.,0.));
#17504=DIRECTION('center_axis',(0.,0.,1.));
#17505=DIRECTION('ref_axis',(1.,0.,0.));
#17506=DIRECTION('',(-1.,0.,0.));
#17507=DIRECTION('',(1.,0.,0.));
#17508=DIRECTION('',(0.,1.,0.));
#17509=DIRECTION('center_axis',(-0.939692620785908,0.,0.342020143325669));
#17510=DIRECTION('ref_axis',(0.342020143325669,0.,0.939692620785908));
#17511=DIRECTION('',(-0.342020143325669,0.,-0.939692620785908));
#17512=DIRECTION('',(0.342020143325669,0.,0.939692620785908));
#17513=DIRECTION('',(0.,1.,0.));
#17514=DIRECTION('center_axis',(0.,0.,1.));
#17515=DIRECTION('ref_axis',(1.,0.,0.));
#17516=DIRECTION('',(-1.,0.,0.));
#17517=DIRECTION('',(1.,0.,0.));
#17518=DIRECTION('',(0.,1.,0.));
#17519=DIRECTION('center_axis',(0.939692620785908,0.,0.342020143325669));
#17520=DIRECTION('ref_axis',(0.342020143325669,0.,-0.939692620785908));
#17521=DIRECTION('',(-0.342020143325669,0.,0.939692620785908));
#17522=DIRECTION('',(0.342020143325669,0.,-0.939692620785908));
#17523=DIRECTION('',(0.,1.,0.));
#17524=DIRECTION('center_axis',(0.,0.,1.));
#17525=DIRECTION('ref_axis',(1.,0.,0.));
#17526=DIRECTION('',(-1.,0.,0.));
#17527=DIRECTION('',(1.,0.,0.));
#17528=DIRECTION('',(0.,1.,0.));
#17529=DIRECTION('center_axis',(-0.939692620785908,0.,0.342020143325669));
#17530=DIRECTION('ref_axis',(0.342020143325669,0.,0.939692620785908));
#17531=DIRECTION('',(-0.342020143325669,0.,-0.939692620785908));
#17532=DIRECTION('',(0.342020143325669,0.,0.939692620785908));
#17533=DIRECTION('',(0.,1.,0.));
#17534=DIRECTION('center_axis',(0.,0.,1.));
#17535=DIRECTION('ref_axis',(1.,0.,0.));
#17536=DIRECTION('',(-1.,0.,0.));
#17537=DIRECTION('',(1.,0.,0.));
#17538=DIRECTION('',(0.,1.,0.));
#17539=DIRECTION('center_axis',(0.939692620785908,0.,0.342020143325669));
#17540=DIRECTION('ref_axis',(0.342020143325669,0.,-0.939692620785908));
#17541=DIRECTION('',(-0.342020143325669,0.,0.939692620785908));
#17542=DIRECTION('',(0.342020143325669,0.,-0.939692620785908));
#17543=DIRECTION('',(0.,1.,0.));
#17544=DIRECTION('center_axis',(0.,0.,1.));
#17545=DIRECTION('ref_axis',(1.,0.,0.));
#17546=DIRECTION('',(-1.,0.,0.));
#17547=DIRECTION('',(1.,0.,0.));
#17548=DIRECTION('',(0.,1.,0.));
#17549=DIRECTION('center_axis',(-0.939692620785908,0.,0.342020143325669));
#17550=DIRECTION('ref_axis',(0.342020143325669,0.,0.939692620785908));
#17551=DIRECTION('',(-0.342020143325669,0.,-0.939692620785908));
#17552=DIRECTION('',(0.342020143325669,0.,0.939692620785908));
#17553=DIRECTION('',(0.,1.,0.));
#17554=DIRECTION('center_axis',(0.,0.,1.));
#17555=DIRECTION('ref_axis',(1.,0.,0.));
#17556=DIRECTION('',(-1.,0.,0.));
#17557=DIRECTION('',(1.,0.,0.));
#17558=DIRECTION('',(0.,1.,0.));
#17559=DIRECTION('center_axis',(0.939692620785908,0.,0.342020143325669));
#17560=DIRECTION('ref_axis',(0.342020143325669,0.,-0.939692620785908));
#17561=DIRECTION('',(-0.342020143325669,0.,0.939692620785908));
#17562=DIRECTION('',(0.342020143325669,0.,-0.939692620785908));
#17563=DIRECTION('',(0.,1.,0.));
#17564=DIRECTION('center_axis',(0.,0.,1.));
#17565=DIRECTION('ref_axis',(1.,0.,0.));
#17566=DIRECTION('',(-1.,0.,0.));
#17567=DIRECTION('',(1.,0.,0.));
#17568=DIRECTION('',(0.,1.,0.));
#17569=DIRECTION('center_axis',(-0.939692620785908,0.,0.342020143325669));
#17570=DIRECTION('ref_axis',(0.342020143325669,0.,0.939692620785908));
#17571=DIRECTION('',(-0.342020143325669,0.,-0.939692620785908));
#17572=DIRECTION('',(0.342020143325669,0.,0.939692620785908));
#17573=DIRECTION('',(0.,1.,0.));
#17574=DIRECTION('center_axis',(0.,0.,1.));
#17575=DIRECTION('ref_axis',(1.,0.,0.));
#17576=DIRECTION('',(-1.,0.,0.));
#17577=DIRECTION('',(1.,0.,0.));
#17578=DIRECTION('',(0.,1.,0.));
#17579=DIRECTION('center_axis',(0.939692620785908,0.,0.342020143325669));
#17580=DIRECTION('ref_axis',(0.342020143325669,0.,-0.939692620785908));
#17581=DIRECTION('',(-0.342020143325669,0.,0.939692620785908));
#17582=DIRECTION('',(0.342020143325669,0.,-0.939692620785908));
#17583=DIRECTION('',(0.,1.,0.));
#17584=DIRECTION('center_axis',(0.,0.,1.));
#17585=DIRECTION('ref_axis',(1.,0.,0.));
#17586=DIRECTION('',(-1.,0.,0.));
#17587=DIRECTION('',(1.,0.,0.));
#17588=DIRECTION('',(0.,1.,0.));
#17589=DIRECTION('center_axis',(-0.939692620785908,0.,0.342020143325669));
#17590=DIRECTION('ref_axis',(0.342020143325669,0.,0.939692620785908));
#17591=DIRECTION('',(-0.342020143325669,0.,-0.939692620785908));
#17592=DIRECTION('',(0.342020143325669,0.,0.939692620785908));
#17593=DIRECTION('',(0.,1.,0.));
#17594=DIRECTION('center_axis',(0.,0.,1.));
#17595=DIRECTION('ref_axis',(1.,0.,0.));
#17596=DIRECTION('',(-1.,0.,0.));
#17597=DIRECTION('',(1.,0.,0.));
#17598=DIRECTION('',(0.,1.,0.));
#17599=DIRECTION('center_axis',(0.939692620785908,0.,0.342020143325669));
#17600=DIRECTION('ref_axis',(0.342020143325669,0.,-0.939692620785908));
#17601=DIRECTION('',(-0.342020143325669,0.,0.939692620785908));
#17602=DIRECTION('',(0.342020143325669,0.,-0.939692620785908));
#17603=DIRECTION('',(0.,1.,0.));
#17604=DIRECTION('center_axis',(0.,0.,1.));
#17605=DIRECTION('ref_axis',(1.,0.,0.));
#17606=DIRECTION('',(-1.,0.,0.));
#17607=DIRECTION('',(1.,0.,0.));
#17608=DIRECTION('',(0.,1.,0.));
#17609=DIRECTION('center_axis',(-0.939692620785911,0.,0.342020143325662));
#17610=DIRECTION('ref_axis',(0.342020143325662,0.,0.939692620785911));
#17611=DIRECTION('',(-0.342020143325662,0.,-0.939692620785911));
#17612=DIRECTION('',(0.342020143325662,0.,0.939692620785911));
#17613=DIRECTION('',(0.,1.,0.));
#17614=DIRECTION('center_axis',(0.,0.,1.));
#17615=DIRECTION('ref_axis',(1.,0.,0.));
#17616=DIRECTION('',(-1.,0.,0.));
#17617=DIRECTION('',(1.,0.,0.));
#17618=DIRECTION('',(0.,1.,0.));
#17619=DIRECTION('center_axis',(0.939692620785908,0.,0.342020143325669));
#17620=DIRECTION('ref_axis',(0.342020143325669,0.,-0.939692620785908));
#17621=DIRECTION('',(-0.342020143325669,0.,0.939692620785908));
#17622=DIRECTION('',(0.342020143325669,0.,-0.939692620785908));
#17623=DIRECTION('',(0.,1.,0.));
#17624=DIRECTION('center_axis',(0.,0.,1.));
#17625=DIRECTION('ref_axis',(1.,0.,0.));
#17626=DIRECTION('',(-1.,0.,0.));
#17627=DIRECTION('',(1.,0.,0.));
#17628=DIRECTION('',(0.,1.,0.));
#17629=DIRECTION('center_axis',(-0.939692620785908,0.,0.342020143325669));
#17630=DIRECTION('ref_axis',(0.342020143325669,0.,0.939692620785908));
#17631=DIRECTION('',(-0.342020143325669,0.,-0.939692620785908));
#17632=DIRECTION('',(0.342020143325669,0.,0.939692620785908));
#17633=DIRECTION('',(0.,1.,0.));
#17634=DIRECTION('center_axis',(0.,0.,1.));
#17635=DIRECTION('ref_axis',(1.,0.,0.));
#17636=DIRECTION('',(-1.,0.,0.));
#17637=DIRECTION('',(1.,0.,0.));
#17638=DIRECTION('',(0.,1.,0.));
#17639=DIRECTION('center_axis',(0.93969262078591,0.,0.342020143325665));
#17640=DIRECTION('ref_axis',(0.342020143325665,0.,-0.93969262078591));
#17641=DIRECTION('',(-0.342020143325665,0.,0.93969262078591));
#17642=DIRECTION('',(0.342020143325665,0.,-0.93969262078591));
#17643=DIRECTION('',(0.,1.,0.));
#17644=DIRECTION('center_axis',(0.,0.,1.));
#17645=DIRECTION('ref_axis',(1.,0.,0.));
#17646=DIRECTION('',(-1.,0.,0.));
#17647=DIRECTION('',(1.,0.,0.));
#17648=DIRECTION('',(0.,1.,0.));
#17649=DIRECTION('center_axis',(-0.939692620785908,0.,0.342020143325669));
#17650=DIRECTION('ref_axis',(0.342020143325669,0.,0.939692620785908));
#17651=DIRECTION('',(-0.342020143325669,0.,-0.939692620785908));
#17652=DIRECTION('',(0.342020143325669,0.,0.939692620785908));
#17653=DIRECTION('',(0.,1.,0.));
#17654=DIRECTION('center_axis',(0.,0.,1.));
#17655=DIRECTION('ref_axis',(1.,0.,0.));
#17656=DIRECTION('',(-1.,0.,0.));
#17657=DIRECTION('',(1.,0.,0.));
#17658=DIRECTION('',(0.,1.,0.));
#17659=DIRECTION('center_axis',(0.939692620785908,0.,0.342020143325669));
#17660=DIRECTION('ref_axis',(0.342020143325669,0.,-0.939692620785908));
#17661=DIRECTION('',(-0.342020143325669,0.,0.939692620785908));
#17662=DIRECTION('',(0.342020143325669,0.,-0.939692620785908));
#17663=DIRECTION('',(0.,1.,0.));
#17664=DIRECTION('center_axis',(0.,0.,1.));
#17665=DIRECTION('ref_axis',(1.,0.,0.));
#17666=DIRECTION('',(-1.,0.,0.));
#17667=DIRECTION('',(1.,0.,0.));
#17668=DIRECTION('',(0.,1.,0.));
#17669=DIRECTION('center_axis',(-0.93969262078591,0.,0.342020143325665));
#17670=DIRECTION('ref_axis',(0.342020143325665,0.,0.93969262078591));
#17671=DIRECTION('',(-0.342020143325665,0.,-0.93969262078591));
#17672=DIRECTION('',(0.342020143325665,0.,0.93969262078591));
#17673=DIRECTION('',(0.,1.,0.));
#17674=DIRECTION('center_axis',(0.,0.,1.));
#17675=DIRECTION('ref_axis',(1.,0.,0.));
#17676=DIRECTION('',(-1.,0.,0.));
#17677=DIRECTION('',(1.,0.,0.));
#17678=DIRECTION('',(0.,1.,0.));
#17679=DIRECTION('center_axis',(0.93969262078591,0.,0.342020143325665));
#17680=DIRECTION('ref_axis',(0.342020143325665,0.,-0.93969262078591));
#17681=DIRECTION('',(-0.342020143325665,0.,0.93969262078591));
#17682=DIRECTION('',(0.342020143325665,0.,-0.93969262078591));
#17683=DIRECTION('',(0.,1.,0.));
#17684=DIRECTION('center_axis',(0.,0.,1.));
#17685=DIRECTION('ref_axis',(1.,0.,0.));
#17686=DIRECTION('',(-1.,0.,0.));
#17687=DIRECTION('',(1.,0.,0.));
#17688=DIRECTION('',(0.,1.,0.));
#17689=DIRECTION('center_axis',(-0.93969262078591,0.,0.342020143325665));
#17690=DIRECTION('ref_axis',(0.342020143325665,0.,0.93969262078591));
#17691=DIRECTION('',(-0.342020143325665,0.,-0.93969262078591));
#17692=DIRECTION('',(0.342020143325665,0.,0.93969262078591));
#17693=DIRECTION('',(0.,1.,0.));
#17694=DIRECTION('center_axis',(0.,0.,1.));
#17695=DIRECTION('ref_axis',(1.,0.,0.));
#17696=DIRECTION('',(-1.,0.,0.));
#17697=DIRECTION('',(1.,0.,0.));
#17698=DIRECTION('',(0.,1.,0.));
#17699=DIRECTION('center_axis',(0.939692620785908,0.,0.342020143325669));
#17700=DIRECTION('ref_axis',(0.342020143325669,0.,-0.939692620785908));
#17701=DIRECTION('',(-0.342020143325669,0.,0.939692620785908));
#17702=DIRECTION('',(0.342020143325669,0.,-0.939692620785908));
#17703=DIRECTION('',(0.,1.,0.));
#17704=DIRECTION('center_axis',(0.,0.,1.));
#17705=DIRECTION('ref_axis',(1.,0.,0.));
#17706=DIRECTION('',(-1.,0.,0.));
#17707=DIRECTION('',(1.,0.,0.));
#17708=DIRECTION('',(0.,1.,0.));
#17709=DIRECTION('center_axis',(-0.939692620785908,0.,0.342020143325669));
#17710=DIRECTION('ref_axis',(0.342020143325669,0.,0.939692620785908));
#17711=DIRECTION('',(-0.342020143325669,0.,-0.939692620785908));
#17712=DIRECTION('',(0.342020143325669,0.,0.939692620785908));
#17713=DIRECTION('',(0.,1.,0.));
#17714=DIRECTION('center_axis',(0.,0.,1.));
#17715=DIRECTION('ref_axis',(1.,0.,0.));
#17716=DIRECTION('',(-1.,0.,0.));
#17717=DIRECTION('',(1.,0.,0.));
#17718=DIRECTION('',(0.,1.,0.));
#17719=DIRECTION('center_axis',(0.93969262078591,0.,0.342020143325665));
#17720=DIRECTION('ref_axis',(0.342020143325665,0.,-0.93969262078591));
#17721=DIRECTION('',(-0.342020143325665,0.,0.93969262078591));
#17722=DIRECTION('',(0.342020143325665,0.,-0.93969262078591));
#17723=DIRECTION('',(0.,1.,0.));
#17724=DIRECTION('center_axis',(0.,0.,1.));
#17725=DIRECTION('ref_axis',(1.,0.,0.));
#17726=DIRECTION('',(-1.,0.,0.));
#17727=DIRECTION('',(1.,0.,0.));
#17728=DIRECTION('',(0.,1.,0.));
#17729=DIRECTION('center_axis',(-0.939692620785907,0.,0.342020143325672));
#17730=DIRECTION('ref_axis',(0.342020143325672,0.,0.939692620785907));
#17731=DIRECTION('',(-0.342020143325672,0.,-0.939692620785907));
#17732=DIRECTION('',(0.342020143325672,0.,0.939692620785907));
#17733=DIRECTION('',(0.,1.,0.));
#17734=DIRECTION('center_axis',(0.,0.,1.));
#17735=DIRECTION('ref_axis',(1.,0.,0.));
#17736=DIRECTION('',(-1.,0.,0.));
#17737=DIRECTION('',(1.,0.,0.));
#17738=DIRECTION('',(0.,1.,0.));
#17739=DIRECTION('center_axis',(0.939692620785907,0.,0.342020143325672));
#17740=DIRECTION('ref_axis',(0.342020143325672,0.,-0.939692620785907));
#17741=DIRECTION('',(-0.342020143325672,0.,0.939692620785907));
#17742=DIRECTION('',(0.342020143325672,0.,-0.939692620785907));
#17743=DIRECTION('',(0.,1.,0.));
#17744=DIRECTION('center_axis',(0.,0.,1.));
#17745=DIRECTION('ref_axis',(1.,0.,0.));
#17746=DIRECTION('',(-1.,0.,0.));
#17747=DIRECTION('',(1.,0.,0.));
#17748=DIRECTION('',(0.,1.,0.));
#17749=DIRECTION('center_axis',(-0.939692620785908,0.,0.342020143325669));
#17750=DIRECTION('ref_axis',(0.342020143325669,0.,0.939692620785908));
#17751=DIRECTION('',(-0.342020143325669,0.,-0.939692620785908));
#17752=DIRECTION('',(0.342020143325669,0.,0.939692620785908));
#17753=DIRECTION('',(0.,1.,0.));
#17754=DIRECTION('center_axis',(0.,0.,1.));
#17755=DIRECTION('ref_axis',(1.,0.,0.));
#17756=DIRECTION('',(-1.,0.,0.));
#17757=DIRECTION('',(1.,0.,0.));
#17758=DIRECTION('',(0.,1.,0.));
#17759=DIRECTION('center_axis',(0.939692620785908,0.,0.342020143325669));
#17760=DIRECTION('ref_axis',(0.342020143325669,0.,-0.939692620785908));
#17761=DIRECTION('',(-0.342020143325669,0.,0.939692620785908));
#17762=DIRECTION('',(0.342020143325669,0.,-0.939692620785908));
#17763=DIRECTION('',(0.,1.,0.));
#17764=DIRECTION('center_axis',(0.,0.,1.));
#17765=DIRECTION('ref_axis',(1.,0.,0.));
#17766=DIRECTION('',(-1.,0.,0.));
#17767=DIRECTION('',(1.,0.,0.));
#17768=DIRECTION('',(0.,1.,0.));
#17769=DIRECTION('center_axis',(-0.939692620785907,0.,0.342020143325672));
#17770=DIRECTION('ref_axis',(0.342020143325672,0.,0.939692620785907));
#17771=DIRECTION('',(-0.342020143325672,0.,-0.939692620785907));
#17772=DIRECTION('',(0.342020143325672,0.,0.939692620785907));
#17773=DIRECTION('',(0.,1.,0.));
#17774=DIRECTION('center_axis',(0.,0.,1.));
#17775=DIRECTION('ref_axis',(1.,0.,0.));
#17776=DIRECTION('',(-1.,0.,0.));
#17777=DIRECTION('',(1.,0.,0.));
#17778=DIRECTION('',(0.,1.,0.));
#17779=DIRECTION('center_axis',(0.939692620785907,0.,0.342020143325672));
#17780=DIRECTION('ref_axis',(0.342020143325672,0.,-0.939692620785907));
#17781=DIRECTION('',(-0.342020143325672,0.,0.939692620785907));
#17782=DIRECTION('',(0.342020143325672,0.,-0.939692620785907));
#17783=DIRECTION('',(0.,1.,0.));
#17784=DIRECTION('center_axis',(0.,0.,1.));
#17785=DIRECTION('ref_axis',(1.,0.,0.));
#17786=DIRECTION('',(-1.,0.,0.));
#17787=DIRECTION('',(1.,0.,0.));
#17788=DIRECTION('',(0.,1.,0.));
#17789=DIRECTION('center_axis',(-0.939692620785908,0.,0.342020143325669));
#17790=DIRECTION('ref_axis',(0.342020143325669,0.,0.939692620785908));
#17791=DIRECTION('',(-0.342020143325669,0.,-0.939692620785908));
#17792=DIRECTION('',(0.342020143325669,0.,0.939692620785908));
#17793=DIRECTION('',(0.,1.,0.));
#17794=DIRECTION('center_axis',(0.,0.,1.));
#17795=DIRECTION('ref_axis',(1.,0.,0.));
#17796=DIRECTION('',(-1.,0.,0.));
#17797=DIRECTION('',(1.,0.,0.));
#17798=DIRECTION('',(0.,1.,0.));
#17799=DIRECTION('center_axis',(0.939692620785908,0.,0.342020143325669));
#17800=DIRECTION('ref_axis',(0.342020143325669,0.,-0.939692620785908));
#17801=DIRECTION('',(-0.342020143325669,0.,0.939692620785908));
#17802=DIRECTION('',(0.342020143325669,0.,-0.939692620785908));
#17803=DIRECTION('',(0.,1.,0.));
#17804=DIRECTION('center_axis',(0.,0.,1.));
#17805=DIRECTION('ref_axis',(1.,0.,0.));
#17806=DIRECTION('',(-1.,0.,0.));
#17807=DIRECTION('',(1.,0.,0.));
#17808=DIRECTION('',(0.,1.,0.));
#17809=DIRECTION('center_axis',(-0.939692620785907,0.,0.342020143325672));
#17810=DIRECTION('ref_axis',(0.342020143325672,0.,0.939692620785907));
#17811=DIRECTION('',(-0.342020143325672,0.,-0.939692620785907));
#17812=DIRECTION('',(0.342020143325672,0.,0.939692620785907));
#17813=DIRECTION('',(0.,1.,0.));
#17814=DIRECTION('center_axis',(0.,0.,1.));
#17815=DIRECTION('ref_axis',(1.,0.,0.));
#17816=DIRECTION('',(-1.,0.,0.));
#17817=DIRECTION('',(1.,0.,0.));
#17818=DIRECTION('',(0.,1.,0.));
#17819=DIRECTION('center_axis',(0.939692620785907,0.,0.342020143325672));
#17820=DIRECTION('ref_axis',(0.342020143325672,0.,-0.939692620785907));
#17821=DIRECTION('',(-0.342020143325672,0.,0.939692620785907));
#17822=DIRECTION('',(0.342020143325672,0.,-0.939692620785907));
#17823=DIRECTION('',(0.,1.,0.));
#17824=DIRECTION('center_axis',(0.,0.,1.));
#17825=DIRECTION('ref_axis',(1.,0.,0.));
#17826=DIRECTION('',(-1.,0.,0.));
#17827=DIRECTION('',(1.,0.,0.));
#17828=DIRECTION('',(0.,1.,0.));
#17829=DIRECTION('center_axis',(-0.939692620785908,0.,0.342020143325669));
#17830=DIRECTION('ref_axis',(0.342020143325669,0.,0.939692620785908));
#17831=DIRECTION('',(-0.342020143325669,0.,-0.939692620785908));
#17832=DIRECTION('',(0.342020143325669,0.,0.939692620785908));
#17833=DIRECTION('',(0.,1.,0.));
#17834=DIRECTION('center_axis',(0.,0.,1.));
#17835=DIRECTION('ref_axis',(1.,0.,0.));
#17836=DIRECTION('',(-1.,0.,0.));
#17837=DIRECTION('',(1.,0.,0.));
#17838=DIRECTION('',(0.,1.,0.));
#17839=DIRECTION('center_axis',(0.939692620785908,0.,0.342020143325669));
#17840=DIRECTION('ref_axis',(0.342020143325669,0.,-0.939692620785908));
#17841=DIRECTION('',(-0.342020143325669,0.,0.939692620785908));
#17842=DIRECTION('',(0.342020143325669,0.,-0.939692620785908));
#17843=DIRECTION('',(0.,1.,0.));
#17844=DIRECTION('center_axis',(0.,0.,1.));
#17845=DIRECTION('ref_axis',(1.,0.,0.));
#17846=DIRECTION('',(-1.,0.,0.));
#17847=DIRECTION('',(1.,0.,0.));
#17848=DIRECTION('',(0.,1.,0.));
#17849=DIRECTION('center_axis',(-0.939692620785907,0.,0.342020143325672));
#17850=DIRECTION('ref_axis',(0.342020143325672,0.,0.939692620785907));
#17851=DIRECTION('',(-0.342020143325672,0.,-0.939692620785907));
#17852=DIRECTION('',(0.342020143325672,0.,0.939692620785907));
#17853=DIRECTION('',(0.,1.,0.));
#17854=DIRECTION('center_axis',(0.,0.,1.));
#17855=DIRECTION('ref_axis',(1.,0.,0.));
#17856=DIRECTION('',(-1.,0.,0.));
#17857=DIRECTION('',(1.,0.,0.));
#17858=DIRECTION('',(0.,1.,0.));
#17859=DIRECTION('center_axis',(0.939692620785907,0.,0.342020143325672));
#17860=DIRECTION('ref_axis',(0.342020143325672,0.,-0.939692620785907));
#17861=DIRECTION('',(-0.342020143325672,0.,0.939692620785907));
#17862=DIRECTION('',(0.342020143325672,0.,-0.939692620785907));
#17863=DIRECTION('',(0.,1.,0.));
#17864=DIRECTION('center_axis',(0.,0.,1.));
#17865=DIRECTION('ref_axis',(1.,0.,0.));
#17866=DIRECTION('',(-1.,0.,0.));
#17867=DIRECTION('',(1.,0.,0.));
#17868=DIRECTION('',(0.,1.,0.));
#17869=DIRECTION('center_axis',(-0.939692620785908,0.,0.34202014332567));
#17870=DIRECTION('ref_axis',(0.34202014332567,0.,0.939692620785908));
#17871=DIRECTION('',(-0.34202014332567,0.,-0.939692620785908));
#17872=DIRECTION('',(0.34202014332567,0.,0.939692620785908));
#17873=DIRECTION('',(0.,1.,0.));
#17874=DIRECTION('center_axis',(0.,0.,1.));
#17875=DIRECTION('ref_axis',(1.,0.,0.));
#17876=DIRECTION('',(-1.,0.,0.));
#17877=DIRECTION('',(1.,0.,0.));
#17878=DIRECTION('',(0.,1.,0.));
#17879=DIRECTION('center_axis',(0.939692620785908,0.,0.342020143325669));
#17880=DIRECTION('ref_axis',(0.342020143325669,0.,-0.939692620785908));
#17881=DIRECTION('',(-0.342020143325669,0.,0.939692620785908));
#17882=DIRECTION('',(0.342020143325669,0.,-0.939692620785908));
#17883=DIRECTION('',(0.,1.,0.));
#17884=DIRECTION('center_axis',(0.,0.,1.));
#17885=DIRECTION('ref_axis',(1.,0.,0.));
#17886=DIRECTION('',(-1.,0.,0.));
#17887=DIRECTION('',(1.,0.,0.));
#17888=DIRECTION('',(0.,1.,0.));
#17889=DIRECTION('center_axis',(-0.939692620785908,0.,0.34202014332567));
#17890=DIRECTION('ref_axis',(0.34202014332567,0.,0.939692620785908));
#17891=DIRECTION('',(-0.34202014332567,0.,-0.939692620785908));
#17892=DIRECTION('',(0.34202014332567,0.,0.939692620785908));
#17893=DIRECTION('',(0.,1.,0.));
#17894=DIRECTION('center_axis',(0.,0.,1.));
#17895=DIRECTION('ref_axis',(1.,0.,0.));
#17896=DIRECTION('',(-1.,0.,0.));
#17897=DIRECTION('',(1.,0.,0.));
#17898=DIRECTION('',(0.,1.,0.));
#17899=DIRECTION('center_axis',(0.939692620785908,0.,0.34202014332567));
#17900=DIRECTION('ref_axis',(0.34202014332567,0.,-0.939692620785908));
#17901=DIRECTION('',(-0.34202014332567,0.,0.939692620785908));
#17902=DIRECTION('',(0.34202014332567,0.,-0.939692620785908));
#17903=DIRECTION('',(0.,1.,0.));
#17904=DIRECTION('center_axis',(0.,0.,1.));
#17905=DIRECTION('ref_axis',(1.,0.,0.));
#17906=DIRECTION('',(-1.,0.,0.));
#17907=DIRECTION('',(1.,0.,0.));
#17908=DIRECTION('',(0.,1.,0.));
#17909=DIRECTION('center_axis',(-0.939692620785908,0.,0.342020143325669));
#17910=DIRECTION('ref_axis',(0.342020143325669,0.,0.939692620785908));
#17911=DIRECTION('',(-0.342020143325669,0.,-0.939692620785908));
#17912=DIRECTION('',(0.342020143325669,0.,0.939692620785908));
#17913=DIRECTION('',(0.,1.,0.));
#17914=DIRECTION('center_axis',(0.,0.,1.));
#17915=DIRECTION('ref_axis',(1.,0.,0.));
#17916=DIRECTION('',(-1.,0.,0.));
#17917=DIRECTION('',(1.,0.,0.));
#17918=DIRECTION('',(0.,1.,0.));
#17919=DIRECTION('center_axis',(0.939692620785908,0.,0.342020143325669));
#17920=DIRECTION('ref_axis',(0.342020143325669,0.,-0.939692620785908));
#17921=DIRECTION('',(-0.342020143325669,0.,0.939692620785908));
#17922=DIRECTION('',(0.342020143325669,0.,-0.939692620785908));
#17923=DIRECTION('',(0.,1.,0.));
#17924=DIRECTION('center_axis',(0.,0.,1.));
#17925=DIRECTION('ref_axis',(1.,0.,0.));
#17926=DIRECTION('',(-1.,0.,0.));
#17927=DIRECTION('',(1.,0.,0.));
#17928=DIRECTION('',(0.,1.,0.));
#17929=DIRECTION('center_axis',(-0.939692620785908,0.,0.34202014332567));
#17930=DIRECTION('ref_axis',(0.34202014332567,0.,0.939692620785908));
#17931=DIRECTION('',(-0.34202014332567,0.,-0.939692620785908));
#17932=DIRECTION('',(0.34202014332567,0.,0.939692620785908));
#17933=DIRECTION('',(0.,1.,0.));
#17934=DIRECTION('center_axis',(0.,0.,1.));
#17935=DIRECTION('ref_axis',(1.,0.,0.));
#17936=DIRECTION('',(-1.,0.,0.));
#17937=DIRECTION('',(1.,0.,0.));
#17938=DIRECTION('',(0.,1.,0.));
#17939=DIRECTION('center_axis',(0.939692620785908,0.,0.342020143325669));
#17940=DIRECTION('ref_axis',(0.342020143325669,0.,-0.939692620785908));
#17941=DIRECTION('',(-0.342020143325669,0.,0.939692620785908));
#17942=DIRECTION('',(0.342020143325669,0.,-0.939692620785908));
#17943=DIRECTION('',(0.,1.,0.));
#17944=DIRECTION('center_axis',(0.,0.,1.));
#17945=DIRECTION('ref_axis',(1.,0.,0.));
#17946=DIRECTION('',(-1.,0.,0.));
#17947=DIRECTION('',(1.,0.,0.));
#17948=DIRECTION('',(0.,1.,0.));
#17949=DIRECTION('center_axis',(-0.939692620785908,0.,0.34202014332567));
#17950=DIRECTION('ref_axis',(0.34202014332567,0.,0.939692620785908));
#17951=DIRECTION('',(-0.34202014332567,0.,-0.939692620785908));
#17952=DIRECTION('',(0.34202014332567,0.,0.939692620785908));
#17953=DIRECTION('',(0.,1.,0.));
#17954=DIRECTION('center_axis',(0.,0.,1.));
#17955=DIRECTION('ref_axis',(1.,0.,0.));
#17956=DIRECTION('',(-1.,0.,0.));
#17957=DIRECTION('',(1.,0.,0.));
#17958=DIRECTION('',(0.,1.,0.));
#17959=DIRECTION('center_axis',(0.939692620785908,0.,0.342020143325669));
#17960=DIRECTION('ref_axis',(0.342020143325669,0.,-0.939692620785908));
#17961=DIRECTION('',(-0.342020143325669,0.,0.939692620785908));
#17962=DIRECTION('',(0.342020143325669,0.,-0.939692620785908));
#17963=DIRECTION('',(0.,1.,0.));
#17964=DIRECTION('center_axis',(0.,0.,1.));
#17965=DIRECTION('ref_axis',(1.,0.,0.));
#17966=DIRECTION('',(-1.,0.,0.));
#17967=DIRECTION('',(1.,0.,0.));
#17968=DIRECTION('',(0.,1.,0.));
#17969=DIRECTION('center_axis',(-0.939692620785908,0.,0.34202014332567));
#17970=DIRECTION('ref_axis',(0.34202014332567,0.,0.939692620785908));
#17971=DIRECTION('',(-0.34202014332567,0.,-0.939692620785908));
#17972=DIRECTION('',(0.34202014332567,0.,0.939692620785908));
#17973=DIRECTION('',(0.,1.,0.));
#17974=DIRECTION('center_axis',(0.,0.,1.));
#17975=DIRECTION('ref_axis',(1.,0.,0.));
#17976=DIRECTION('',(-1.,0.,0.));
#17977=DIRECTION('',(1.,0.,0.));
#17978=DIRECTION('',(0.,1.,0.));
#17979=DIRECTION('center_axis',(0.939692620785908,0.,0.34202014332567));
#17980=DIRECTION('ref_axis',(0.34202014332567,0.,-0.939692620785908));
#17981=DIRECTION('',(-0.34202014332567,0.,0.939692620785908));
#17982=DIRECTION('',(0.34202014332567,0.,-0.939692620785908));
#17983=DIRECTION('',(0.,1.,0.));
#17984=DIRECTION('center_axis',(0.,0.,1.));
#17985=DIRECTION('ref_axis',(1.,0.,0.));
#17986=DIRECTION('',(-1.,0.,0.));
#17987=DIRECTION('',(1.,0.,0.));
#17988=DIRECTION('',(0.,1.,0.));
#17989=DIRECTION('center_axis',(-0.939692620785908,0.,0.34202014332567));
#17990=DIRECTION('ref_axis',(0.34202014332567,0.,0.939692620785908));
#17991=DIRECTION('',(-0.34202014332567,0.,-0.939692620785908));
#17992=DIRECTION('',(0.34202014332567,0.,0.939692620785908));
#17993=DIRECTION('',(0.,1.,0.));
#17994=DIRECTION('center_axis',(0.,0.,1.));
#17995=DIRECTION('ref_axis',(1.,0.,0.));
#17996=DIRECTION('',(-1.,0.,0.));
#17997=DIRECTION('',(1.,0.,0.));
#17998=DIRECTION('',(0.,1.,0.));
#17999=DIRECTION('center_axis',(0.939692620785908,0.,0.342020143325669));
#18000=DIRECTION('ref_axis',(0.342020143325669,0.,-0.939692620785908));
#18001=DIRECTION('',(-0.342020143325669,0.,0.939692620785908));
#18002=DIRECTION('',(0.342020143325669,0.,-0.939692620785908));
#18003=DIRECTION('',(0.,1.,0.));
#18004=DIRECTION('center_axis',(0.,0.,1.));
#18005=DIRECTION('ref_axis',(1.,0.,0.));
#18006=DIRECTION('',(-1.,0.,0.));
#18007=DIRECTION('',(1.,0.,0.));
#18008=DIRECTION('',(0.,1.,0.));
#18009=DIRECTION('center_axis',(-0.939692620785908,0.,0.342020143325669));
#18010=DIRECTION('ref_axis',(0.342020143325669,0.,0.939692620785908));
#18011=DIRECTION('',(-0.342020143325669,0.,-0.939692620785908));
#18012=DIRECTION('',(0.342020143325669,0.,0.939692620785908));
#18013=DIRECTION('',(0.,1.,0.));
#18014=DIRECTION('center_axis',(0.,0.,1.));
#18015=DIRECTION('ref_axis',(1.,0.,0.));
#18016=DIRECTION('',(-1.,0.,0.));
#18017=DIRECTION('',(1.,0.,0.));
#18018=DIRECTION('',(0.,1.,0.));
#18019=DIRECTION('center_axis',(0.939692620785908,0.,0.342020143325669));
#18020=DIRECTION('ref_axis',(0.342020143325669,0.,-0.939692620785908));
#18021=DIRECTION('',(-0.342020143325669,0.,0.939692620785908));
#18022=DIRECTION('',(0.342020143325669,0.,-0.939692620785908));
#18023=DIRECTION('',(0.,1.,0.));
#18024=DIRECTION('center_axis',(0.,0.,1.));
#18025=DIRECTION('ref_axis',(1.,0.,0.));
#18026=DIRECTION('',(-1.,0.,0.));
#18027=DIRECTION('',(1.,0.,0.));
#18028=DIRECTION('',(0.,1.,0.));
#18029=DIRECTION('center_axis',(-0.939692620785908,0.,0.342020143325669));
#18030=DIRECTION('ref_axis',(0.342020143325669,0.,0.939692620785908));
#18031=DIRECTION('',(-0.342020143325669,0.,-0.939692620785908));
#18032=DIRECTION('',(0.342020143325669,0.,0.939692620785908));
#18033=DIRECTION('',(0.,1.,0.));
#18034=DIRECTION('center_axis',(0.,0.,1.));
#18035=DIRECTION('ref_axis',(1.,0.,0.));
#18036=DIRECTION('',(-1.,0.,0.));
#18037=DIRECTION('',(1.,0.,0.));
#18038=DIRECTION('',(0.,1.,0.));
#18039=DIRECTION('center_axis',(0.939692620785908,0.,0.342020143325669));
#18040=DIRECTION('ref_axis',(0.342020143325669,0.,-0.939692620785908));
#18041=DIRECTION('',(-0.342020143325669,0.,0.939692620785908));
#18042=DIRECTION('',(0.342020143325669,0.,-0.939692620785908));
#18043=DIRECTION('',(0.,1.,0.));
#18044=DIRECTION('center_axis',(0.,0.,1.));
#18045=DIRECTION('ref_axis',(1.,0.,0.));
#18046=DIRECTION('',(-1.,0.,0.));
#18047=DIRECTION('',(1.,0.,0.));
#18048=DIRECTION('',(0.,1.,0.));
#18049=DIRECTION('center_axis',(-0.939692620785908,0.,0.342020143325669));
#18050=DIRECTION('ref_axis',(0.342020143325669,0.,0.939692620785908));
#18051=DIRECTION('',(-0.342020143325669,0.,-0.939692620785908));
#18052=DIRECTION('',(0.342020143325669,0.,0.939692620785908));
#18053=DIRECTION('',(0.,1.,0.));
#18054=DIRECTION('center_axis',(0.,0.,1.));
#18055=DIRECTION('ref_axis',(1.,0.,0.));
#18056=DIRECTION('',(-1.,0.,0.));
#18057=DIRECTION('',(1.,0.,0.));
#18058=DIRECTION('',(0.,1.,0.));
#18059=DIRECTION('center_axis',(0.939692620785908,0.,0.342020143325669));
#18060=DIRECTION('ref_axis',(0.342020143325669,0.,-0.939692620785908));
#18061=DIRECTION('',(-0.342020143325669,0.,0.939692620785908));
#18062=DIRECTION('',(0.342020143325669,0.,-0.939692620785908));
#18063=DIRECTION('',(0.,1.,0.));
#18064=DIRECTION('center_axis',(0.,0.,1.));
#18065=DIRECTION('ref_axis',(1.,0.,0.));
#18066=DIRECTION('',(-1.,0.,0.));
#18067=DIRECTION('',(1.,0.,0.));
#18068=DIRECTION('',(0.,1.,0.));
#18069=DIRECTION('center_axis',(-0.939692620785908,0.,0.342020143325669));
#18070=DIRECTION('ref_axis',(0.342020143325669,0.,0.939692620785908));
#18071=DIRECTION('',(-0.342020143325669,0.,-0.939692620785908));
#18072=DIRECTION('',(0.342020143325669,0.,0.939692620785908));
#18073=DIRECTION('',(0.,1.,0.));
#18074=DIRECTION('center_axis',(0.,0.,1.));
#18075=DIRECTION('ref_axis',(1.,0.,0.));
#18076=DIRECTION('',(-1.,0.,0.));
#18077=DIRECTION('',(1.,0.,0.));
#18078=DIRECTION('center_axis',(0.,1.,0.));
#18079=DIRECTION('ref_axis',(0.,0.,1.));
#18080=DIRECTION('center_axis',(0.,1.,0.));
#18081=DIRECTION('ref_axis',(1.,0.,0.));
#18082=DIRECTION('axis',(0.,0.,1.));
#18083=DIRECTION('refdir',(1.,0.,0.));
#18084=DIRECTION('axis',(0.,0.,1.));
#18085=DIRECTION('refdir',(1.,0.,0.));
#18086=DIRECTION('center_axis',(0.,0.,1.));
#18087=DIRECTION('ref_axis',(1.,0.,0.));
#18088=DIRECTION('',(-1.,0.,0.));
#18089=DIRECTION('center_axis',(0.,0.,1.));
#18090=DIRECTION('ref_axis',(1.,0.,0.));
#18091=DIRECTION('center_axis',(0.,0.,1.));
#18092=DIRECTION('ref_axis',(1.,0.,0.));
#18093=DIRECTION('',(0.,0.,-1.));
#18094=DIRECTION('center_axis',(0.,0.,1.));
#18095=DIRECTION('ref_axis',(1.,0.,0.));
#18096=DIRECTION('',(0.,0.,1.));
#18097=DIRECTION('center_axis',(0.,0.,-1.));
#18098=DIRECTION('ref_axis',(1.,0.,0.));
#18099=DIRECTION('center_axis',(0.,0.,1.));
#18100=DIRECTION('ref_axis',(1.,0.,0.));
#18101=DIRECTION('',(0.,0.,1.));
#18102=DIRECTION('center_axis',(0.,0.,1.));
#18103=DIRECTION('ref_axis',(1.,0.,0.));
#18104=DIRECTION('',(1.,0.,0.));
#18105=DIRECTION('center_axis',(0.,0.,1.));
#18106=DIRECTION('ref_axis',(1.,0.,0.));
#18107=DIRECTION('center_axis',(0.,0.,1.));
#18108=DIRECTION('ref_axis',(1.,0.,0.));
#18109=DIRECTION('',(0.,0.,-1.));
#18110=DIRECTION('center_axis',(0.,0.,1.));
#18111=DIRECTION('ref_axis',(1.,0.,0.));
#18112=DIRECTION('',(0.,0.,1.));
#18113=DIRECTION('center_axis',(0.,0.,-1.));
#18114=DIRECTION('ref_axis',(1.,0.,0.));
#18115=DIRECTION('center_axis',(0.,0.,1.));
#18116=DIRECTION('ref_axis',(1.,0.,0.));
#18117=DIRECTION('',(0.,0.,1.));
#18118=DIRECTION('center_axis',(0.,0.,1.));
#18119=DIRECTION('ref_axis',(1.,0.,0.));
#18120=DIRECTION('',(-1.,0.,0.));
#18121=DIRECTION('center_axis',(0.,0.,1.));
#18122=DIRECTION('ref_axis',(1.,0.,0.));
#18123=DIRECTION('center_axis',(0.,0.,1.));
#18124=DIRECTION('ref_axis',(1.,0.,0.));
#18125=DIRECTION('',(0.,0.,-1.));
#18126=DIRECTION('center_axis',(0.,0.,1.));
#18127=DIRECTION('ref_axis',(1.,0.,0.));
#18128=DIRECTION('',(0.,0.,1.));
#18129=DIRECTION('center_axis',(0.,0.,-1.));
#18130=DIRECTION('ref_axis',(1.,0.,0.));
#18131=DIRECTION('center_axis',(0.,0.,1.));
#18132=DIRECTION('ref_axis',(1.,0.,0.));
#18133=DIRECTION('',(0.,0.,1.));
#18134=DIRECTION('center_axis',(0.,0.,1.));
#18135=DIRECTION('ref_axis',(1.,0.,0.));
#18136=DIRECTION('',(1.,0.,0.));
#18137=DIRECTION('center_axis',(0.,0.,1.));
#18138=DIRECTION('ref_axis',(1.,0.,0.));
#18139=DIRECTION('center_axis',(0.,0.,1.));
#18140=DIRECTION('ref_axis',(1.,0.,0.));
#18141=DIRECTION('',(0.,0.,-1.));
#18142=DIRECTION('center_axis',(0.,0.,1.));
#18143=DIRECTION('ref_axis',(1.,0.,0.));
#18144=DIRECTION('',(0.,0.,1.));
#18145=DIRECTION('center_axis',(0.,0.,-1.));
#18146=DIRECTION('ref_axis',(1.,0.,0.));
#18147=DIRECTION('center_axis',(0.,0.,1.));
#18148=DIRECTION('ref_axis',(1.,0.,0.));
#18149=DIRECTION('',(0.,0.,1.));
#18150=DIRECTION('center_axis',(0.,-1.,0.));
#18151=DIRECTION('ref_axis',(0.,0.,-1.));
#18152=DIRECTION('',(-1.,0.,0.));
#18153=DIRECTION('',(-1.,0.,0.));
#18154=DIRECTION('',(0.,0.,1.));
#18155=DIRECTION('',(1.,0.,0.));
#18156=DIRECTION('',(0.,0.,-1.));
#18157=DIRECTION('',(-1.,0.,0.));
#18158=DIRECTION('center_axis',(0.,1.,0.));
#18159=DIRECTION('ref_axis',(0.,0.,1.));
#18160=DIRECTION('',(1.,0.,0.));
#18161=DIRECTION('',(1.,0.,0.));
#18162=DIRECTION('',(0.,0.,1.));
#18163=DIRECTION('',(1.,0.,0.));
#18164=DIRECTION('',(0.,0.,-1.));
#18165=DIRECTION('',(1.,0.,0.));
#18166=DIRECTION('center_axis',(-1.,0.,0.));
#18167=DIRECTION('ref_axis',(0.,0.,1.));
#18168=DIRECTION('',(0.,-1.,0.));
#18169=DIRECTION('',(0.,0.,1.));
#18170=DIRECTION('',(0.,1.,0.));
#18171=DIRECTION('',(0.,0.,-1.));
#18172=DIRECTION('',(0.,-1.,0.));
#18173=DIRECTION('',(0.,-1.,0.));
#18174=DIRECTION('',(0.,0.,1.));
#18175=DIRECTION('',(0.,-1.,0.));
#18176=DIRECTION('',(0.,0.,-1.));
#18177=DIRECTION('',(0.,-1.,0.));
#18178=DIRECTION('center_axis',(0.,0.,-1.));
#18179=DIRECTION('ref_axis',(0.,1.,0.));
#18180=DIRECTION('',(0.,1.,0.));
#18181=DIRECTION('',(1.,0.,0.));
#18182=DIRECTION('center_axis',(0.,-1.,0.));
#18183=DIRECTION('ref_axis',(0.,0.,-1.));
#18184=DIRECTION('',(0.,0.,-1.));
#18185=DIRECTION('',(1.,0.,0.));
#18186=DIRECTION('center_axis',(0.,0.,1.));
#18187=DIRECTION('ref_axis',(0.,-1.,0.));
#18188=DIRECTION('',(0.,-1.,0.));
#18189=DIRECTION('',(1.,0.,0.));
#18190=DIRECTION('center_axis',(0.,1.,0.));
#18191=DIRECTION('ref_axis',(0.,0.,1.));
#18192=DIRECTION('',(0.,0.,1.));
#18193=DIRECTION('',(1.,0.,0.));
#18194=DIRECTION('center_axis',(0.,0.,-1.));
#18195=DIRECTION('ref_axis',(0.,1.,0.));
#18196=DIRECTION('',(0.,1.,0.));
#18197=DIRECTION('center_axis',(0.,0.,-1.));
#18198=DIRECTION('ref_axis',(0.,1.,0.));
#18199=DIRECTION('',(0.,1.,0.));
#18200=DIRECTION('',(1.,0.,0.));
#18201=DIRECTION('center_axis',(0.,-1.,0.));
#18202=DIRECTION('ref_axis',(0.,0.,-1.));
#18203=DIRECTION('',(0.,0.,-1.));
#18204=DIRECTION('',(1.,0.,0.));
#18205=DIRECTION('center_axis',(0.,0.,-1.));
#18206=DIRECTION('ref_axis',(0.,1.,0.));
#18207=DIRECTION('',(0.,1.,0.));
#18208=DIRECTION('',(1.,0.,0.));
#18209=DIRECTION('center_axis',(0.,1.,0.));
#18210=DIRECTION('ref_axis',(0.,0.,1.));
#18211=DIRECTION('',(0.,0.,1.));
#18212=DIRECTION('',(1.,0.,0.));
#18213=DIRECTION('center_axis',(0.,0.,-1.));
#18214=DIRECTION('ref_axis',(0.,1.,0.));
#18215=DIRECTION('',(0.,1.,0.));
#18216=DIRECTION('center_axis',(1.,0.,0.));
#18217=DIRECTION('ref_axis',(0.,0.,-1.));
#18218=DIRECTION('axis',(0.,0.,1.));
#18219=DIRECTION('refdir',(1.,0.,0.));
#18220=DIRECTION('center_axis',(0.,0.,1.));
#18221=DIRECTION('ref_axis',(0.,-1.,0.));
#18222=DIRECTION('',(0.,-1.,0.));
#18223=DIRECTION('',(1.,0.,0.));
#18224=DIRECTION('',(0.,-1.,0.));
#18225=DIRECTION('',(1.,0.,0.));
#18226=DIRECTION('center_axis',(0.,1.,0.));
#18227=DIRECTION('ref_axis',(0.,0.,1.));
#18228=DIRECTION('',(0.,0.,1.));
#18229=DIRECTION('',(0.,0.,1.));
#18230=DIRECTION('',(1.,0.,0.));
#18231=DIRECTION('center_axis',(0.,0.,-1.));
#18232=DIRECTION('ref_axis',(0.,1.,0.));
#18233=DIRECTION('',(0.,1.,0.));
#18234=DIRECTION('',(0.,1.,0.));
#18235=DIRECTION('',(1.,0.,0.));
#18236=DIRECTION('center_axis',(0.,-1.,0.));
#18237=DIRECTION('ref_axis',(0.,0.,-1.));
#18238=DIRECTION('',(0.,0.,-1.));
#18239=DIRECTION('',(0.,0.,-1.));
#18240=DIRECTION('',(1.,0.,0.));
#18241=DIRECTION('center_axis',(0.,0.,-1.));
#18242=DIRECTION('ref_axis',(0.,1.,0.));
#18243=DIRECTION('',(0.,1.,0.));
#18244=DIRECTION('',(0.,1.,0.));
#18245=DIRECTION('',(1.,0.,0.));
#18246=DIRECTION('center_axis',(0.,1.,0.));
#18247=DIRECTION('ref_axis',(0.,0.,1.));
#18248=DIRECTION('',(0.,0.,1.));
#18249=DIRECTION('',(0.,0.,1.));
#18250=DIRECTION('',(1.,0.,0.));
#18251=DIRECTION('center_axis',(0.,0.,-1.));
#18252=DIRECTION('ref_axis',(0.,1.,0.));
#18253=DIRECTION('',(0.,1.,0.));
#18254=DIRECTION('',(0.,1.,0.));
#18255=DIRECTION('',(1.,0.,0.));
#18256=DIRECTION('center_axis',(0.,-1.,0.));
#18257=DIRECTION('ref_axis',(0.,0.,-1.));
#18258=DIRECTION('',(0.,0.,-1.));
#18259=DIRECTION('',(0.,0.,-1.));
#18260=DIRECTION('center_axis',(1.,0.,0.));
#18261=DIRECTION('ref_axis',(0.,0.,-1.));
#18262=DIRECTION('center_axis',(1.,0.,0.));
#18263=DIRECTION('ref_axis',(0.,0.,-1.));
#18264=DIRECTION('axis',(0.,0.,1.));
#18265=DIRECTION('refdir',(1.,0.,0.));
#18266=DIRECTION('center_axis',(0.,0.,-1.));
#18267=DIRECTION('ref_axis',(0.,-1.,0.));
#18268=DIRECTION('',(0.,1.,0.));
#18269=DIRECTION('',(-1.,0.,0.));
#18270=DIRECTION('',(0.,-1.,0.));
#18271=DIRECTION('',(-1.,0.,0.));
#18272=DIRECTION('center_axis',(0.,1.,0.));
#18273=DIRECTION('ref_axis',(0.,0.,-1.));
#18274=DIRECTION('',(0.,0.,1.));
#18275=DIRECTION('',(0.,0.,-1.));
#18276=DIRECTION('',(-1.,0.,0.));
#18277=DIRECTION('center_axis',(0.,0.,-1.));
#18278=DIRECTION('ref_axis',(0.,-1.,0.));
#18279=DIRECTION('',(0.,1.,0.));
#18280=DIRECTION('',(0.,-1.,0.));
#18281=DIRECTION('',(-1.,0.,0.));
#18282=DIRECTION('center_axis',(0.,-1.,0.));
#18283=DIRECTION('ref_axis',(0.,0.,1.));
#18284=DIRECTION('',(0.,0.,-1.));
#18285=DIRECTION('',(0.,0.,1.));
#18286=DIRECTION('',(-1.,0.,0.));
#18287=DIRECTION('center_axis',(0.,0.,-1.));
#18288=DIRECTION('ref_axis',(0.,-1.,0.));
#18289=DIRECTION('',(0.,1.,0.));
#18290=DIRECTION('',(0.,-1.,0.));
#18291=DIRECTION('',(-1.,0.,0.));
#18292=DIRECTION('center_axis',(0.,1.,0.));
#18293=DIRECTION('ref_axis',(0.,0.,-1.));
#18294=DIRECTION('',(0.,0.,1.));
#18295=DIRECTION('',(0.,0.,-1.));
#18296=DIRECTION('',(-1.,0.,0.));
#18297=DIRECTION('center_axis',(0.,0.,1.));
#18298=DIRECTION('ref_axis',(0.,1.,0.));
#18299=DIRECTION('',(0.,-1.,0.));
#18300=DIRECTION('',(0.,1.,0.));
#18301=DIRECTION('',(-1.,0.,0.));
#18302=DIRECTION('center_axis',(0.,-1.,0.));
#18303=DIRECTION('ref_axis',(0.,0.,1.));
#18304=DIRECTION('',(0.,0.,-1.));
#18305=DIRECTION('',(0.,0.,1.));
#18306=DIRECTION('center_axis',(1.,0.,0.));
#18307=DIRECTION('ref_axis',(0.,0.,-1.));
#18308=DIRECTION('center_axis',(-1.,0.,0.));
#18309=DIRECTION('ref_axis',(0.,0.,1.));
#18310=DIRECTION('',(0.,0.,1.));
#18311=DIRECTION('',(1.,0.,0.));
#18312=DIRECTION('',(0.,0.,1.));
#18313=DIRECTION('',(1.,0.,0.));
#18314=DIRECTION('',(0.,0.,1.));
#18315=DIRECTION('',(1.,0.,0.));
#18316=DIRECTION('axis',(0.,0.,1.));
#18317=DIRECTION('refdir',(1.,0.,0.));
#18318=DIRECTION('center_axis',(0.866025403784439,0.,-0.5));
#18319=DIRECTION('ref_axis',(0.5,0.,0.866025403784439));
#18320=DIRECTION('',(-0.5,0.,-0.866025403784439));
#18321=DIRECTION('',(0.,-1.,0.));
#18322=DIRECTION('',(0.5,0.,0.866025403784439));
#18323=DIRECTION('',(0.,-1.,0.));
#18324=DIRECTION('center_axis',(1.20185167898973E-16,0.,-1.));
#18325=DIRECTION('ref_axis',(1.,0.,1.20185167898973E-16));
#18326=DIRECTION('',(-1.,0.,-1.20185167898973E-16));
#18327=DIRECTION('',(0.,-1.,0.));
#18328=DIRECTION('',(1.,0.,1.20185167898973E-16));
#18329=DIRECTION('center_axis',(-0.866025403784439,0.,-0.5));
#18330=DIRECTION('ref_axis',(0.5,0.,-0.866025403784439));
#18331=DIRECTION('',(-0.5,0.,0.866025403784439));
#18332=DIRECTION('',(0.,-1.,0.));
#18333=DIRECTION('',(0.5,0.,-0.866025403784439));
#18334=DIRECTION('center_axis',(-0.866025403784439,0.,0.5));
#18335=DIRECTION('ref_axis',(-0.5,0.,-0.866025403784439));
#18336=DIRECTION('',(0.5,0.,0.866025403784439));
#18337=DIRECTION('',(0.,-1.,0.));
#18338=DIRECTION('',(-0.5,0.,-0.866025403784439));
#18339=DIRECTION('center_axis',(-2.40370335797945E-16,0.,1.));
#18340=DIRECTION('ref_axis',(-1.,0.,-2.40370335797945E-16));
#18341=DIRECTION('',(1.,0.,2.40370335797945E-16));
#18342=DIRECTION('',(0.,-1.,0.));
#18343=DIRECTION('',(-1.,0.,-2.40370335797945E-16));
#18344=DIRECTION('center_axis',(0.866025403784439,0.,0.5));
#18345=DIRECTION('ref_axis',(-0.5,0.,0.866025403784439));
#18346=DIRECTION('',(0.5,0.,-0.866025403784439));
#18347=DIRECTION('',(-0.5,0.,0.866025403784439));
#18348=DIRECTION('center_axis',(0.,1.,0.));
#18349=DIRECTION('ref_axis',(1.,0.,0.));
#18350=DIRECTION('center_axis',(0.,-1.,0.));
#18351=DIRECTION('ref_axis',(0.,0.,-1.));
#18352=DIRECTION('center_axis',(0.,1.,0.));
#18353=DIRECTION('ref_axis',(1.,0.,0.));
#18354=DIRECTION('center_axis',(0.,1.,0.));
#18355=DIRECTION('ref_axis',(1.,0.,0.));
#18356=DIRECTION('center_axis',(0.,1.,0.));
#18357=DIRECTION('ref_axis',(0.,0.,1.));
#18358=DIRECTION('center_axis',(0.,-1.,0.));
#18359=DIRECTION('ref_axis',(1.,0.,0.));
#18360=DIRECTION('center_axis',(0.,-1.,0.));
#18361=DIRECTION('ref_axis',(1.,0.,0.));
#18362=DIRECTION('center_axis',(0.,-1.,0.));
#18363=DIRECTION('ref_axis',(1.,0.,0.));
#18364=DIRECTION('',(0.707106781186548,0.707106781186547,8.65956056235493E-17));
#18365=DIRECTION('center_axis',(0.,-1.,0.));
#18366=DIRECTION('ref_axis',(1.,0.,0.));
#18367=DIRECTION('center_axis',(0.,-1.,0.));
#18368=DIRECTION('ref_axis',(1.,0.,0.));
#18369=DIRECTION('',(0.,1.,0.));
#18370=DIRECTION('center_axis',(0.,1.,0.));
#18371=DIRECTION('ref_axis',(1.,0.,0.));
#18372=DIRECTION('center_axis',(0.,-1.,0.));
#18373=DIRECTION('ref_axis',(1.,0.,0.));
#18374=DIRECTION('',(-0.707106781186547,0.707106781186548,-8.65956056235493E-17));
#18375=DIRECTION('center_axis',(0.,-1.,0.));
#18376=DIRECTION('ref_axis',(0.,0.,-1.));
#18377=DIRECTION('center_axis',(0.,-1.,0.));
#18378=DIRECTION('ref_axis',(1.,0.,0.));
#18379=DIRECTION('center_axis',(0.,1.,0.));
#18380=DIRECTION('ref_axis',(1.,0.,0.));
#18381=DIRECTION('center_axis',(0.,1.,0.));
#18382=DIRECTION('ref_axis',(1.,0.,0.));
#18383=DIRECTION('',(-0.447213595499958,0.894427190999916,-5.47678698264203E-17));
#18384=DIRECTION('center_axis',(0.,-1.,0.));
#18385=DIRECTION('ref_axis',(1.,0.,0.));
#18386=DIRECTION('',(0.,1.,0.));
#18387=DIRECTION('axis',(0.,0.,1.));
#18388=DIRECTION('refdir',(1.,0.,0.));
#18389=DIRECTION('axis',(0.,0.,1.));
#18390=DIRECTION('refdir',(1.,0.,0.));
#18391=DIRECTION('center_axis',(-1.,0.,0.));
#18392=DIRECTION('ref_axis',(0.,0.,1.));
#18393=DIRECTION('',(0.,-1.,0.));
#18394=DIRECTION('',(0.,0.,1.));
#18395=DIRECTION('',(0.,1.,0.));
#18396=DIRECTION('',(0.,0.,-1.));
#18397=DIRECTION('center_axis',(0.,1.,0.));
#18398=DIRECTION('ref_axis',(1.,0.,0.));
#18399=DIRECTION('center_axis',(0.,-1.,0.));
#18400=DIRECTION('ref_axis',(1.,0.,0.));
#18401=DIRECTION('',(-1.,0.,0.));
#18402=DIRECTION('',(0.,0.,1.));
#18403=DIRECTION('center_axis',(1.,0.,0.));
#18404=DIRECTION('ref_axis',(0.,0.,-1.));
#18405=DIRECTION('',(0.,1.,0.));
#18406=DIRECTION('',(0.,1.,0.));
#18407=DIRECTION('',(0.,0.,-1.));
#18408=DIRECTION('center_axis',(0.,0.,1.));
#18409=DIRECTION('ref_axis',(1.,0.,0.));
#18410=DIRECTION('',(1.,0.,0.));
#18411=DIRECTION('center_axis',(0.,1.,0.));
#18412=DIRECTION('ref_axis',(0.,0.,1.));
#18413=DIRECTION('center_axis',(0.,1.,0.));
#18414=DIRECTION('ref_axis',(1.,0.,0.));
#18415=DIRECTION('center_axis',(0.,1.,0.));
#18416=DIRECTION('ref_axis',(1.,0.,0.));
#18417=DIRECTION('center_axis',(0.,1.,0.));
#18418=DIRECTION('ref_axis',(1.,0.,0.));
#18419=DIRECTION('',(0.,1.,0.));
#18420=DIRECTION('center_axis',(0.,-1.,0.));
#18421=DIRECTION('ref_axis',(1.,0.,0.));
#18422=DIRECTION('center_axis',(0.,1.,0.));
#18423=DIRECTION('ref_axis',(1.,0.,0.));
#18424=DIRECTION('center_axis',(0.,1.,0.));
#18425=DIRECTION('ref_axis',(1.,0.,0.));
#18426=DIRECTION('center_axis',(0.,1.,0.));
#18427=DIRECTION('ref_axis',(1.,0.,0.));
#18428=DIRECTION('',(0.,1.,0.));
#18429=DIRECTION('center_axis',(0.,1.,0.));
#18430=DIRECTION('ref_axis',(1.,0.,0.));
#18431=DIRECTION('center_axis',(0.,1.,0.));
#18432=DIRECTION('ref_axis',(1.,0.,0.));
#18433=DIRECTION('center_axis',(-1.,0.,0.));
#18434=DIRECTION('ref_axis',(0.,0.,1.));
#18435=DIRECTION('',(0.,-1.,0.));
#18436=DIRECTION('',(0.,0.,1.));
#18437=DIRECTION('',(0.,1.,0.));
#18438=DIRECTION('',(0.,0.,-1.));
#18439=DIRECTION('center_axis',(0.,1.,0.));
#18440=DIRECTION('ref_axis',(1.,0.,0.));
#18441=DIRECTION('center_axis',(0.,-1.,0.));
#18442=DIRECTION('ref_axis',(1.,0.,0.));
#18443=DIRECTION('',(-1.,0.,0.));
#18444=DIRECTION('',(0.,0.,1.));
#18445=DIRECTION('center_axis',(1.,0.,0.));
#18446=DIRECTION('ref_axis',(0.,0.,-1.));
#18447=DIRECTION('',(0.,1.,0.));
#18448=DIRECTION('',(0.,1.,0.));
#18449=DIRECTION('',(0.,0.,-1.));
#18450=DIRECTION('center_axis',(0.,0.,1.));
#18451=DIRECTION('ref_axis',(1.,0.,0.));
#18452=DIRECTION('',(1.,0.,0.));
#18453=DIRECTION('center_axis',(0.,1.,0.));
#18454=DIRECTION('ref_axis',(0.,0.,1.));
#18455=DIRECTION('center_axis',(0.,1.,0.));
#18456=DIRECTION('ref_axis',(1.,0.,0.));
#18457=DIRECTION('center_axis',(0.,1.,0.));
#18458=DIRECTION('ref_axis',(1.,0.,0.));
#18459=DIRECTION('center_axis',(0.,1.,0.));
#18460=DIRECTION('ref_axis',(1.,0.,0.));
#18461=DIRECTION('center_axis',(0.,1.,0.));
#18462=DIRECTION('ref_axis',(1.,0.,0.));
#18463=DIRECTION('center_axis',(0.,1.,0.));
#18464=DIRECTION('ref_axis',(1.,0.,0.));
#18465=DIRECTION('center_axis',(0.,1.,0.));
#18466=DIRECTION('ref_axis',(1.,0.,0.));
#18467=DIRECTION('center_axis',(0.,-1.,0.));
#18468=DIRECTION('ref_axis',(1.,0.,0.));
#18469=DIRECTION('center_axis',(0.,1.,0.));
#18470=DIRECTION('ref_axis',(1.,0.,0.));
#18471=DIRECTION('',(0.,-1.,0.));
#18472=DIRECTION('center_axis',(0.,1.,0.));
#18473=DIRECTION('ref_axis',(1.,0.,0.));
#18474=DIRECTION('',(0.,-1.,0.));
#18475=DIRECTION('center_axis',(0.,1.,0.));
#18476=DIRECTION('ref_axis',(1.,0.,0.));
#18477=DIRECTION('center_axis',(0.,1.,0.));
#18478=DIRECTION('ref_axis',(1.,0.,0.));
#18479=DIRECTION('center_axis',(0.,1.,0.));
#18480=DIRECTION('ref_axis',(1.,0.,0.));
#18481=DIRECTION('',(0.,-1.,0.));
#18482=DIRECTION('center_axis',(0.,1.,0.));
#18483=DIRECTION('ref_axis',(1.,0.,0.));
#18484=DIRECTION('center_axis',(0.,1.,0.));
#18485=DIRECTION('ref_axis',(1.,0.,0.));
#18486=DIRECTION('axis',(0.,0.,1.));
#18487=DIRECTION('refdir',(1.,0.,0.));
#18488=DIRECTION('center_axis',(0.,1.,0.));
#18489=DIRECTION('ref_axis',(1.,0.,0.));
#18490=DIRECTION('center_axis',(0.,-1.,0.));
#18491=DIRECTION('ref_axis',(1.,0.,0.));
#18492=DIRECTION('',(0.,-1.,0.));
#18493=DIRECTION('center_axis',(0.,-1.,0.));
#18494=DIRECTION('ref_axis',(1.,0.,0.));
#18495=DIRECTION('center_axis',(0.,1.,0.));
#18496=DIRECTION('ref_axis',(1.,0.,0.));
#18497=DIRECTION('center_axis',(0.,1.,0.));
#18498=DIRECTION('ref_axis',(1.,0.,0.));
#18499=DIRECTION('',(0.,-1.,0.));
#18500=DIRECTION('center_axis',(0.,1.,0.));
#18501=DIRECTION('ref_axis',(1.,0.,0.));
#18502=DIRECTION('center_axis',(0.,1.,0.));
#18503=DIRECTION('ref_axis',(1.,0.,0.));
#18504=DIRECTION('center_axis',(0.,1.,0.));
#18505=DIRECTION('ref_axis',(1.,0.,0.));
#18506=DIRECTION('axis',(0.,0.,1.));
#18507=DIRECTION('refdir',(1.,0.,0.));
#18508=DIRECTION('center_axis',(0.,1.,0.));
#18509=DIRECTION('ref_axis',(1.,0.,0.));
#18510=DIRECTION('center_axis',(0.,-1.,0.));
#18511=DIRECTION('ref_axis',(1.,0.,0.));
#18512=DIRECTION('',(0.,-1.,0.));
#18513=DIRECTION('center_axis',(0.,-1.,0.));
#18514=DIRECTION('ref_axis',(1.,0.,0.));
#18515=DIRECTION('center_axis',(0.,1.,0.));
#18516=DIRECTION('ref_axis',(1.,0.,0.));
#18517=DIRECTION('center_axis',(0.,1.,0.));
#18518=DIRECTION('ref_axis',(1.,0.,0.));
#18519=DIRECTION('',(0.,-1.,0.));
#18520=DIRECTION('center_axis',(0.,1.,0.));
#18521=DIRECTION('ref_axis',(1.,0.,0.));
#18522=DIRECTION('center_axis',(0.,1.,0.));
#18523=DIRECTION('ref_axis',(1.,0.,0.));
#18524=DIRECTION('center_axis',(0.,1.,0.));
#18525=DIRECTION('ref_axis',(1.,0.,0.));
#18526=DIRECTION('axis',(0.,0.,1.));
#18527=DIRECTION('refdir',(1.,0.,0.));
#18528=DIRECTION('center_axis',(0.,1.,0.));
#18529=DIRECTION('ref_axis',(1.,0.,0.));
#18530=DIRECTION('center_axis',(0.,-1.,0.));
#18531=DIRECTION('ref_axis',(1.,0.,0.));
#18532=DIRECTION('',(0.,-1.,0.));
#18533=DIRECTION('center_axis',(0.,-1.,0.));
#18534=DIRECTION('ref_axis',(1.,0.,0.));
#18535=DIRECTION('center_axis',(0.,1.,0.));
#18536=DIRECTION('ref_axis',(1.,0.,0.));
#18537=DIRECTION('center_axis',(0.,1.,0.));
#18538=DIRECTION('ref_axis',(1.,0.,0.));
#18539=DIRECTION('',(0.,-1.,0.));
#18540=DIRECTION('center_axis',(0.,1.,0.));
#18541=DIRECTION('ref_axis',(1.,0.,0.));
#18542=DIRECTION('center_axis',(0.,1.,0.));
#18543=DIRECTION('ref_axis',(1.,0.,0.));
#18544=DIRECTION('center_axis',(0.,1.,0.));
#18545=DIRECTION('ref_axis',(1.,0.,0.));
#18546=DIRECTION('axis',(0.,0.,1.));
#18547=DIRECTION('refdir',(1.,0.,0.));
#18548=DIRECTION('center_axis',(0.,1.,0.));
#18549=DIRECTION('ref_axis',(1.,0.,0.));
#18550=DIRECTION('center_axis',(0.,-1.,0.));
#18551=DIRECTION('ref_axis',(1.,0.,0.));
#18552=DIRECTION('',(0.,-1.,0.));
#18553=DIRECTION('center_axis',(0.,-1.,0.));
#18554=DIRECTION('ref_axis',(1.,0.,0.));
#18555=DIRECTION('center_axis',(0.,1.,0.));
#18556=DIRECTION('ref_axis',(1.,0.,0.));
#18557=DIRECTION('center_axis',(0.,1.,0.));
#18558=DIRECTION('ref_axis',(1.,0.,0.));
#18559=DIRECTION('',(0.,-1.,0.));
#18560=DIRECTION('center_axis',(0.,1.,0.));
#18561=DIRECTION('ref_axis',(1.,0.,0.));
#18562=DIRECTION('center_axis',(0.,1.,0.));
#18563=DIRECTION('ref_axis',(1.,0.,0.));
#18564=DIRECTION('center_axis',(0.,1.,0.));
#18565=DIRECTION('ref_axis',(1.,0.,0.));
#18566=DIRECTION('axis',(0.,0.,1.));
#18567=DIRECTION('refdir',(1.,0.,0.));
#18568=DIRECTION('center_axis',(0.,1.,0.));
#18569=DIRECTION('ref_axis',(1.,0.,0.));
#18570=DIRECTION('center_axis',(0.,-1.,0.));
#18571=DIRECTION('ref_axis',(1.,0.,0.));
#18572=DIRECTION('',(0.,-1.,0.));
#18573=DIRECTION('center_axis',(0.,-1.,0.));
#18574=DIRECTION('ref_axis',(1.,0.,0.));
#18575=DIRECTION('center_axis',(0.,1.,0.));
#18576=DIRECTION('ref_axis',(1.,0.,0.));
#18577=DIRECTION('center_axis',(0.,1.,0.));
#18578=DIRECTION('ref_axis',(1.,0.,0.));
#18579=DIRECTION('',(0.,-1.,0.));
#18580=DIRECTION('center_axis',(0.,1.,0.));
#18581=DIRECTION('ref_axis',(1.,0.,0.));
#18582=DIRECTION('center_axis',(0.,1.,0.));
#18583=DIRECTION('ref_axis',(1.,0.,0.));
#18584=DIRECTION('center_axis',(0.,1.,0.));
#18585=DIRECTION('ref_axis',(1.,0.,0.));
#18586=DIRECTION('axis',(0.,0.,1.));
#18587=DIRECTION('refdir',(1.,0.,0.));
#18588=DIRECTION('center_axis',(0.,1.,0.));
#18589=DIRECTION('ref_axis',(1.,0.,0.));
#18590=DIRECTION('center_axis',(0.,-1.,0.));
#18591=DIRECTION('ref_axis',(1.,0.,0.));
#18592=DIRECTION('',(0.,-1.,0.));
#18593=DIRECTION('center_axis',(0.,-1.,0.));
#18594=DIRECTION('ref_axis',(1.,0.,0.));
#18595=DIRECTION('center_axis',(0.,1.,0.));
#18596=DIRECTION('ref_axis',(1.,0.,0.));
#18597=DIRECTION('center_axis',(0.,1.,0.));
#18598=DIRECTION('ref_axis',(1.,0.,0.));
#18599=DIRECTION('',(0.,-1.,0.));
#18600=DIRECTION('center_axis',(0.,1.,0.));
#18601=DIRECTION('ref_axis',(1.,0.,0.));
#18602=DIRECTION('center_axis',(0.,1.,0.));
#18603=DIRECTION('ref_axis',(1.,0.,0.));
#18604=DIRECTION('center_axis',(0.,1.,0.));
#18605=DIRECTION('ref_axis',(1.,0.,0.));
#18606=DIRECTION('axis',(0.,0.,1.));
#18607=DIRECTION('refdir',(1.,0.,0.));
#18608=DIRECTION('center_axis',(0.,1.,0.));
#18609=DIRECTION('ref_axis',(1.,0.,0.));
#18610=DIRECTION('center_axis',(0.,1.,0.));
#18611=DIRECTION('ref_axis',(1.,0.,0.));
#18612=DIRECTION('',(0.,1.,0.));
#18613=DIRECTION('center_axis',(0.,-1.,0.));
#18614=DIRECTION('ref_axis',(1.,0.,0.));
#18615=DIRECTION('center_axis',(-1.,0.,0.));
#18616=DIRECTION('ref_axis',(0.,0.,1.));
#18617=DIRECTION('',(0.,0.,1.));
#18618=DIRECTION('',(0.,1.,0.));
#18619=DIRECTION('',(0.,0.,-1.));
#18620=DIRECTION('',(0.,1.,0.));
#18621=DIRECTION('center_axis',(0.,0.,-1.));
#18622=DIRECTION('ref_axis',(-1.,0.,0.));
#18623=DIRECTION('',(-1.,0.,0.));
#18624=DIRECTION('',(0.,1.,0.));
#18625=DIRECTION('',(1.,0.,0.));
#18626=DIRECTION('center_axis',(1.,0.,0.));
#18627=DIRECTION('ref_axis',(0.,0.,-1.));
#18628=DIRECTION('',(0.,0.,-1.));
#18629=DIRECTION('',(0.,-1.,0.));
#18630=DIRECTION('',(0.,0.,1.));
#18631=DIRECTION('center_axis',(0.,1.,0.));
#18632=DIRECTION('ref_axis',(1.,0.,0.));
#18633=DIRECTION('center_axis',(0.,1.,0.));
#18634=DIRECTION('ref_axis',(1.,0.,0.));
#18635=DIRECTION('center_axis',(0.,-1.,0.));
#18636=DIRECTION('ref_axis',(1.,0.,0.));
#18637=DIRECTION('center_axis',(0.,1.,0.));
#18638=DIRECTION('ref_axis',(-1.83697019872103E-16,0.,1.));
#18639=DIRECTION('center_axis',(0.,-1.,0.));
#18640=DIRECTION('ref_axis',(1.,0.,0.));
#18641=DIRECTION('center_axis',(0.,1.,0.));
#18642=DIRECTION('ref_axis',(6.12323399573677E-17,0.,1.));
#18643=DIRECTION('',(0.,-1.,0.));
#18644=DIRECTION('center_axis',(0.,1.,0.));
#18645=DIRECTION('ref_axis',(1.,0.,0.));
#18646=DIRECTION('',(0.,1.,0.));
#18647=DIRECTION('center_axis',(0.,1.,0.));
#18648=DIRECTION('ref_axis',(1.,0.,0.));
#18649=DIRECTION('center_axis',(1.,0.,0.));
#18650=DIRECTION('ref_axis',(0.,0.,-1.));
#18651=DIRECTION('',(0.,0.,1.));
#18652=DIRECTION('',(0.,-1.,0.));
#18653=DIRECTION('',(0.,0.,-1.));
#18654=DIRECTION('center_axis',(0.,1.,0.));
#18655=DIRECTION('ref_axis',(1.,0.,0.));
#18656=DIRECTION('',(0.,0.,-1.));
#18657=DIRECTION('center_axis',(0.,-1.,0.));
#18658=DIRECTION('ref_axis',(1.,0.,0.));
#18659=DIRECTION('center_axis',(-1.,0.,0.));
#18660=DIRECTION('ref_axis',(0.,0.,1.));
#18661=DIRECTION('',(0.,0.,1.));
#18662=DIRECTION('',(0.,1.,0.));
#18663=DIRECTION('center_axis',(0.,1.,0.));
#18664=DIRECTION('ref_axis',(0.,0.,1.));
#18665=DIRECTION('center_axis',(0.,1.,0.));
#18666=DIRECTION('ref_axis',(1.,0.,0.));
#18667=DIRECTION('center_axis',(0.,1.,0.));
#18668=DIRECTION('ref_axis',(1.,0.,0.));
#18669=DIRECTION('',(0.,-1.,0.));
#18670=DIRECTION('center_axis',(0.,1.,0.));
#18671=DIRECTION('ref_axis',(1.,0.,0.));
#18672=DIRECTION('center_axis',(0.,1.,0.));
#18673=DIRECTION('ref_axis',(1.,0.,0.));
#18674=DIRECTION('axis',(0.,0.,1.));
#18675=DIRECTION('refdir',(1.,0.,0.));
#18676=DIRECTION('center_axis',(0.,1.,0.));
#18677=DIRECTION('ref_axis',(1.,0.,0.));
#18678=DIRECTION('center_axis',(0.,-1.,0.));
#18679=DIRECTION('ref_axis',(1.,0.,0.));
#18680=DIRECTION('',(0.,-1.,0.));
#18681=DIRECTION('center_axis',(0.,-1.,0.));
#18682=DIRECTION('ref_axis',(1.,0.,0.));
#18683=DIRECTION('center_axis',(0.,1.,0.));
#18684=DIRECTION('ref_axis',(1.,0.,0.));
#18685=DIRECTION('center_axis',(0.,1.,0.));
#18686=DIRECTION('ref_axis',(1.,0.,0.));
#18687=DIRECTION('',(0.,-1.,0.));
#18688=DIRECTION('center_axis',(0.,1.,0.));
#18689=DIRECTION('ref_axis',(1.,0.,0.));
#18690=DIRECTION('center_axis',(0.,1.,0.));
#18691=DIRECTION('ref_axis',(1.,0.,0.));
#18692=DIRECTION('center_axis',(0.,1.,0.));
#18693=DIRECTION('ref_axis',(1.,0.,0.));
#18694=DIRECTION('axis',(0.,0.,1.));
#18695=DIRECTION('refdir',(1.,0.,0.));
#18696=DIRECTION('center_axis',(1.,0.,0.));
#18697=DIRECTION('ref_axis',(0.,0.,-1.));
#18698=DIRECTION('',(0.,0.,1.));
#18699=DIRECTION('',(0.,1.,0.));
#18700=DIRECTION('',(0.,0.,-1.));
#18701=DIRECTION('',(0.,-1.,0.));
#18702=DIRECTION('center_axis',(0.,0.,-1.));
#18703=DIRECTION('ref_axis',(-1.,0.,0.));
#18704=DIRECTION('',(1.,0.,0.));
#18705=DIRECTION('',(0.,-1.,0.));
#18706=DIRECTION('',(-1.,0.,0.));
#18707=DIRECTION('center_axis',(-1.,0.,0.));
#18708=DIRECTION('ref_axis',(0.,0.,1.));
#18709=DIRECTION('',(0.,0.,-1.));
#18710=DIRECTION('',(0.,1.,0.));
#18711=DIRECTION('',(0.,0.,1.));
#18712=DIRECTION('center_axis',(0.,1.,0.));
#18713=DIRECTION('ref_axis',(1.,0.,0.));
#18714=DIRECTION('center_axis',(0.,-1.,0.));
#18715=DIRECTION('ref_axis',(1.,0.,0.));
#18716=DIRECTION('',(-0.587785252292473,0.,0.809016994374947));
#18717=DIRECTION('center_axis',(0.,-1.,0.));
#18718=DIRECTION('ref_axis',(1.,0.,0.));
#18719=DIRECTION('',(-0.809016994374948,0.,0.587785252292473));
#18720=DIRECTION('center_axis',(0.,-1.,0.));
#18721=DIRECTION('ref_axis',(1.,0.,0.));
#18722=DIRECTION('',(-0.951056516295154,0.,0.309016994374947));
#18723=DIRECTION('center_axis',(0.,-1.,0.));
#18724=DIRECTION('ref_axis',(1.,0.,0.));
#18725=DIRECTION('',(-1.,0.,-1.83697019872103E-16));
#18726=DIRECTION('center_axis',(0.,-1.,0.));
#18727=DIRECTION('ref_axis',(1.,0.,0.));
#18728=DIRECTION('',(-0.951056516295154,0.,-0.309016994374948));
#18729=DIRECTION('center_axis',(0.,-1.,0.));
#18730=DIRECTION('ref_axis',(1.,0.,0.));
#18731=DIRECTION('',(-0.809016994374947,0.,-0.587785252292473));
#18732=DIRECTION('center_axis',(0.,-1.,0.));
#18733=DIRECTION('ref_axis',(1.,0.,0.));
#18734=DIRECTION('',(-0.587785252292473,0.,-0.809016994374948));
#18735=DIRECTION('center_axis',(0.,-1.,0.));
#18736=DIRECTION('ref_axis',(1.,0.,0.));
#18737=DIRECTION('',(-0.309016994374947,0.,-0.951056516295154));
#18738=DIRECTION('center_axis',(0.,-1.,0.));
#18739=DIRECTION('ref_axis',(1.,0.,0.));
#18740=DIRECTION('',(1.22464679914735E-16,0.,-1.));
#18741=DIRECTION('center_axis',(0.,-1.,0.));
#18742=DIRECTION('ref_axis',(1.,0.,0.));
#18743=DIRECTION('',(0.309016994374948,0.,-0.951056516295154));
#18744=DIRECTION('center_axis',(0.,-1.,0.));
#18745=DIRECTION('ref_axis',(1.,0.,0.));
#18746=DIRECTION('',(0.587785252292473,0.,-0.809016994374947));
#18747=DIRECTION('center_axis',(0.,-1.,0.));
#18748=DIRECTION('ref_axis',(1.,0.,0.));
#18749=DIRECTION('',(0.809016994374948,0.,-0.587785252292473));
#18750=DIRECTION('center_axis',(0.,-1.,0.));
#18751=DIRECTION('ref_axis',(1.,0.,0.));
#18752=DIRECTION('',(0.951056516295154,0.,-0.309016994374947));
#18753=DIRECTION('center_axis',(0.,-1.,0.));
#18754=DIRECTION('ref_axis',(1.,0.,0.));
#18755=DIRECTION('',(1.,0.,6.12323399573677E-17));
#18756=DIRECTION('center_axis',(0.,-1.,0.));
#18757=DIRECTION('ref_axis',(1.,0.,0.));
#18758=DIRECTION('',(0.951056516295154,0.,0.309016994374948));
#18759=DIRECTION('center_axis',(0.,-1.,0.));
#18760=DIRECTION('ref_axis',(1.,0.,0.));
#18761=DIRECTION('',(0.809016994374947,0.,0.587785252292473));
#18762=DIRECTION('center_axis',(0.,-1.,0.));
#18763=DIRECTION('ref_axis',(1.,0.,0.));
#18764=DIRECTION('',(0.587785252292473,0.,0.809016994374947));
#18765=DIRECTION('center_axis',(0.,-1.,0.));
#18766=DIRECTION('ref_axis',(1.,0.,0.));
#18767=DIRECTION('',(0.309016994374947,0.,0.951056516295154));
#18768=DIRECTION('center_axis',(0.,-1.,0.));
#18769=DIRECTION('ref_axis',(1.,0.,0.));
#18770=DIRECTION('',(0.,0.,1.));
#18771=DIRECTION('center_axis',(0.,-1.,0.));
#18772=DIRECTION('ref_axis',(1.,0.,0.));
#18773=DIRECTION('',(-0.309016994374948,0.,0.951056516295154));
#18774=DIRECTION('center_axis',(0.,1.,0.));
#18775=DIRECTION('ref_axis',(1.,0.,0.));
#18776=DIRECTION('center_axis',(0.,1.,0.));
#18777=DIRECTION('ref_axis',(6.12323399573677E-17,0.,1.));
#18778=DIRECTION('center_axis',(0.,-1.,0.));
#18779=DIRECTION('ref_axis',(1.,0.,0.));
#18780=DIRECTION('center_axis',(0.,1.,0.));
#18781=DIRECTION('ref_axis',(1.,0.,0.));
#18782=DIRECTION('center_axis',(0.,1.,0.));
#18783=DIRECTION('ref_axis',(1.,0.,0.));
#18784=DIRECTION('',(0.,-1.,0.));
#18785=DIRECTION('center_axis',(0.,-1.,0.));
#18786=DIRECTION('ref_axis',(1.,0.,0.));
#18787=DIRECTION('center_axis',(0.,1.,0.));
#18788=DIRECTION('ref_axis',(1.,0.,0.));
#18789=DIRECTION('',(0.,-1.,0.));
#18790=DIRECTION('',(0.,1.,0.));
#18791=DIRECTION('center_axis',(0.951056516295154,0.,0.309016994374948));
#18792=DIRECTION('ref_axis',(0.309016994374948,0.,-0.951056516295154));
#18793=DIRECTION('',(0.309016994374948,0.,-0.951056516295154));
#18794=DIRECTION('',(0.,1.,0.));
#18795=DIRECTION('',(0.,1.,0.));
#18796=DIRECTION('center_axis',(0.,1.,0.));
#18797=DIRECTION('ref_axis',(1.,0.,0.));
#18798=DIRECTION('center_axis',(0.,1.,0.));
#18799=DIRECTION('ref_axis',(1.,0.,0.));
#18800=DIRECTION('',(0.,-1.,0.));
#18801=DIRECTION('',(0.,1.,0.));
#18802=DIRECTION('center_axis',(0.809016994374947,0.,0.587785252292473));
#18803=DIRECTION('ref_axis',(0.587785252292473,0.,-0.809016994374947));
#18804=DIRECTION('',(0.587785252292473,0.,-0.809016994374947));
#18805=DIRECTION('',(0.,1.,0.));
#18806=DIRECTION('',(0.,1.,0.));
#18807=DIRECTION('center_axis',(0.,1.,0.));
#18808=DIRECTION('ref_axis',(1.,0.,0.));
#18809=DIRECTION('center_axis',(0.,1.,0.));
#18810=DIRECTION('ref_axis',(1.,0.,0.));
#18811=DIRECTION('',(0.,-1.,0.));
#18812=DIRECTION('',(0.,1.,0.));
#18813=DIRECTION('center_axis',(0.587785252292473,0.,0.809016994374948));
#18814=DIRECTION('ref_axis',(0.809016994374948,0.,-0.587785252292473));
#18815=DIRECTION('',(0.809016994374948,0.,-0.587785252292473));
#18816=DIRECTION('',(0.,1.,0.));
#18817=DIRECTION('',(0.,1.,0.));
#18818=DIRECTION('center_axis',(0.,1.,0.));
#18819=DIRECTION('ref_axis',(1.,0.,0.));
#18820=DIRECTION('center_axis',(0.,1.,0.));
#18821=DIRECTION('ref_axis',(1.,0.,0.));
#18822=DIRECTION('',(0.,-1.,0.));
#18823=DIRECTION('',(0.,1.,0.));
#18824=DIRECTION('center_axis',(0.309016994374947,0.,0.951056516295154));
#18825=DIRECTION('ref_axis',(0.951056516295154,0.,-0.309016994374947));
#18826=DIRECTION('',(0.951056516295154,0.,-0.309016994374947));
#18827=DIRECTION('',(0.,1.,0.));
#18828=DIRECTION('',(0.,1.,0.));
#18829=DIRECTION('center_axis',(0.,1.,0.));
#18830=DIRECTION('ref_axis',(1.,0.,0.));
#18831=DIRECTION('center_axis',(0.,1.,0.));
#18832=DIRECTION('ref_axis',(1.,0.,0.));
#18833=DIRECTION('',(0.,-1.,0.));
#18834=DIRECTION('',(0.,1.,0.));
#18835=DIRECTION('center_axis',(-1.83697019872103E-16,0.,1.));
#18836=DIRECTION('ref_axis',(1.,0.,1.83697019872103E-16));
#18837=DIRECTION('',(1.,0.,1.83697019872103E-16));
#18838=DIRECTION('',(0.,1.,0.));
#18839=DIRECTION('',(0.,1.,0.));
#18840=DIRECTION('center_axis',(0.,1.,0.));
#18841=DIRECTION('ref_axis',(1.,0.,0.));
#18842=DIRECTION('center_axis',(0.,1.,0.));
#18843=DIRECTION('ref_axis',(1.,0.,0.));
#18844=DIRECTION('',(0.,-1.,0.));
#18845=DIRECTION('',(0.,1.,0.));
#18846=DIRECTION('center_axis',(-0.309016994374948,0.,0.951056516295154));
#18847=DIRECTION('ref_axis',(0.951056516295154,0.,0.309016994374948));
#18848=DIRECTION('',(0.951056516295154,0.,0.309016994374948));
#18849=DIRECTION('',(0.,1.,0.));
#18850=DIRECTION('',(0.,1.,0.));
#18851=DIRECTION('center_axis',(0.,1.,0.));
#18852=DIRECTION('ref_axis',(1.,0.,0.));
#18853=DIRECTION('center_axis',(0.,1.,0.));
#18854=DIRECTION('ref_axis',(1.,0.,0.));
#18855=DIRECTION('',(0.,-1.,0.));
#18856=DIRECTION('',(0.,1.,0.));
#18857=DIRECTION('center_axis',(-0.587785252292473,0.,0.809016994374947));
#18858=DIRECTION('ref_axis',(0.809016994374947,0.,0.587785252292473));
#18859=DIRECTION('',(0.809016994374947,0.,0.587785252292473));
#18860=DIRECTION('',(0.,1.,0.));
#18861=DIRECTION('',(0.,1.,0.));
#18862=DIRECTION('center_axis',(0.,1.,0.));
#18863=DIRECTION('ref_axis',(1.,0.,0.));
#18864=DIRECTION('center_axis',(0.,1.,0.));
#18865=DIRECTION('ref_axis',(1.,0.,0.));
#18866=DIRECTION('',(0.,-1.,0.));
#18867=DIRECTION('',(0.,1.,0.));
#18868=DIRECTION('center_axis',(-0.809016994374948,0.,0.587785252292473));
#18869=DIRECTION('ref_axis',(0.587785252292473,0.,0.809016994374948));
#18870=DIRECTION('',(0.587785252292473,0.,0.809016994374948));
#18871=DIRECTION('',(0.,1.,0.));
#18872=DIRECTION('',(0.,1.,0.));
#18873=DIRECTION('center_axis',(0.,1.,0.));
#18874=DIRECTION('ref_axis',(1.,0.,0.));
#18875=DIRECTION('center_axis',(0.,1.,0.));
#18876=DIRECTION('ref_axis',(1.,0.,0.));
#18877=DIRECTION('',(0.,-1.,0.));
#18878=DIRECTION('',(0.,1.,0.));
#18879=DIRECTION('center_axis',(-0.951056516295154,0.,0.309016994374947));
#18880=DIRECTION('ref_axis',(0.309016994374947,0.,0.951056516295154));
#18881=DIRECTION('',(0.309016994374947,0.,0.951056516295154));
#18882=DIRECTION('',(0.,1.,0.));
#18883=DIRECTION('',(0.,1.,0.));
#18884=DIRECTION('center_axis',(0.,1.,0.));
#18885=DIRECTION('ref_axis',(1.,0.,0.));
#18886=DIRECTION('center_axis',(0.,1.,0.));
#18887=DIRECTION('ref_axis',(1.,0.,0.));
#18888=DIRECTION('',(0.,-1.,0.));
#18889=DIRECTION('',(0.,1.,0.));
#18890=DIRECTION('center_axis',(-1.,0.,-1.22464679914735E-16));
#18891=DIRECTION('ref_axis',(-1.22464679914735E-16,0.,1.));
#18892=DIRECTION('',(-1.22464679914735E-16,0.,1.));
#18893=DIRECTION('',(0.,1.,0.));
#18894=DIRECTION('',(0.,1.,0.));
#18895=DIRECTION('center_axis',(0.,1.,0.));
#18896=DIRECTION('ref_axis',(1.,0.,0.));
#18897=DIRECTION('center_axis',(0.,1.,0.));
#18898=DIRECTION('ref_axis',(1.,0.,0.));
#18899=DIRECTION('',(0.,-1.,0.));
#18900=DIRECTION('',(0.,1.,0.));
#18901=DIRECTION('center_axis',(-0.951056516295154,0.,-0.309016994374948));
#18902=DIRECTION('ref_axis',(-0.309016994374948,0.,0.951056516295154));
#18903=DIRECTION('',(-0.309016994374948,0.,0.951056516295154));
#18904=DIRECTION('',(0.,1.,0.));
#18905=DIRECTION('',(0.,1.,0.));
#18906=DIRECTION('center_axis',(0.,1.,0.));
#18907=DIRECTION('ref_axis',(1.,0.,0.));
#18908=DIRECTION('center_axis',(0.,1.,0.));
#18909=DIRECTION('ref_axis',(1.,0.,0.));
#18910=DIRECTION('',(0.,-1.,0.));
#18911=DIRECTION('',(0.,1.,0.));
#18912=DIRECTION('center_axis',(-0.809016994374947,0.,-0.587785252292473));
#18913=DIRECTION('ref_axis',(-0.587785252292473,0.,0.809016994374947));
#18914=DIRECTION('',(-0.587785252292473,0.,0.809016994374947));
#18915=DIRECTION('',(0.,1.,0.));
#18916=DIRECTION('',(0.,1.,0.));
#18917=DIRECTION('center_axis',(0.,1.,0.));
#18918=DIRECTION('ref_axis',(1.,0.,0.));
#18919=DIRECTION('center_axis',(0.,1.,0.));
#18920=DIRECTION('ref_axis',(1.,0.,0.));
#18921=DIRECTION('',(0.,-1.,0.));
#18922=DIRECTION('',(0.,1.,0.));
#18923=DIRECTION('center_axis',(-0.587785252292473,0.,-0.809016994374948));
#18924=DIRECTION('ref_axis',(-0.809016994374948,0.,0.587785252292473));
#18925=DIRECTION('',(-0.809016994374948,0.,0.587785252292473));
#18926=DIRECTION('',(0.,1.,0.));
#18927=DIRECTION('',(0.,1.,0.));
#18928=DIRECTION('center_axis',(0.,1.,0.));
#18929=DIRECTION('ref_axis',(1.,0.,0.));
#18930=DIRECTION('center_axis',(0.,1.,0.));
#18931=DIRECTION('ref_axis',(1.,0.,0.));
#18932=DIRECTION('',(0.,-1.,0.));
#18933=DIRECTION('',(0.,1.,0.));
#18934=DIRECTION('center_axis',(-0.309016994374947,0.,-0.951056516295154));
#18935=DIRECTION('ref_axis',(-0.951056516295154,0.,0.309016994374947));
#18936=DIRECTION('',(-0.951056516295154,0.,0.309016994374947));
#18937=DIRECTION('',(0.,1.,0.));
#18938=DIRECTION('',(0.,1.,0.));
#18939=DIRECTION('center_axis',(0.,1.,0.));
#18940=DIRECTION('ref_axis',(1.,0.,0.));
#18941=DIRECTION('center_axis',(0.,1.,0.));
#18942=DIRECTION('ref_axis',(1.,0.,0.));
#18943=DIRECTION('',(0.,-1.,0.));
#18944=DIRECTION('',(0.,1.,0.));
#18945=DIRECTION('center_axis',(6.12323399573677E-17,0.,-1.));
#18946=DIRECTION('ref_axis',(-1.,0.,-6.12323399573677E-17));
#18947=DIRECTION('',(-1.,0.,-6.12323399573677E-17));
#18948=DIRECTION('',(0.,1.,0.));
#18949=DIRECTION('',(0.,1.,0.));
#18950=DIRECTION('center_axis',(0.,1.,0.));
#18951=DIRECTION('ref_axis',(1.,0.,0.));
#18952=DIRECTION('center_axis',(0.,1.,0.));
#18953=DIRECTION('ref_axis',(1.,0.,0.));
#18954=DIRECTION('',(0.,-1.,0.));
#18955=DIRECTION('',(0.,1.,0.));
#18956=DIRECTION('center_axis',(0.309016994374948,0.,-0.951056516295154));
#18957=DIRECTION('ref_axis',(-0.951056516295154,0.,-0.309016994374948));
#18958=DIRECTION('',(-0.951056516295154,0.,-0.309016994374948));
#18959=DIRECTION('',(0.,1.,0.));
#18960=DIRECTION('',(0.,1.,0.));
#18961=DIRECTION('center_axis',(0.,1.,0.));
#18962=DIRECTION('ref_axis',(1.,0.,0.));
#18963=DIRECTION('center_axis',(0.,1.,0.));
#18964=DIRECTION('ref_axis',(1.,0.,0.));
#18965=DIRECTION('',(0.,-1.,0.));
#18966=DIRECTION('',(0.,1.,0.));
#18967=DIRECTION('center_axis',(0.587785252292473,0.,-0.809016994374947));
#18968=DIRECTION('ref_axis',(-0.809016994374947,0.,-0.587785252292473));
#18969=DIRECTION('',(-0.809016994374947,0.,-0.587785252292473));
#18970=DIRECTION('',(0.,1.,0.));
#18971=DIRECTION('',(0.,1.,0.));
#18972=DIRECTION('center_axis',(0.,1.,0.));
#18973=DIRECTION('ref_axis',(1.,0.,0.));
#18974=DIRECTION('center_axis',(0.,1.,0.));
#18975=DIRECTION('ref_axis',(1.,0.,0.));
#18976=DIRECTION('',(0.,-1.,0.));
#18977=DIRECTION('',(0.,1.,0.));
#18978=DIRECTION('center_axis',(0.809016994374947,0.,-0.587785252292473));
#18979=DIRECTION('ref_axis',(-0.587785252292473,0.,-0.809016994374947));
#18980=DIRECTION('',(-0.587785252292473,0.,-0.809016994374947));
#18981=DIRECTION('',(0.,1.,0.));
#18982=DIRECTION('',(0.,1.,0.));
#18983=DIRECTION('center_axis',(0.,1.,0.));
#18984=DIRECTION('ref_axis',(1.,0.,0.));
#18985=DIRECTION('center_axis',(0.,1.,0.));
#18986=DIRECTION('ref_axis',(1.,0.,0.));
#18987=DIRECTION('',(0.,-1.,0.));
#18988=DIRECTION('',(0.,1.,0.));
#18989=DIRECTION('center_axis',(0.951056516295154,0.,-0.309016994374947));
#18990=DIRECTION('ref_axis',(-0.309016994374947,0.,-0.951056516295154));
#18991=DIRECTION('',(-0.309016994374947,0.,-0.951056516295154));
#18992=DIRECTION('',(0.,1.,0.));
#18993=DIRECTION('',(0.,1.,0.));
#18994=DIRECTION('center_axis',(0.,1.,0.));
#18995=DIRECTION('ref_axis',(1.,0.,0.));
#18996=DIRECTION('center_axis',(0.,1.,0.));
#18997=DIRECTION('ref_axis',(1.,0.,0.));
#18998=DIRECTION('',(0.,-1.,0.));
#18999=DIRECTION('',(0.,1.,0.));
#19000=DIRECTION('center_axis',(1.,0.,0.));
#19001=DIRECTION('ref_axis',(0.,0.,-1.));
#19002=DIRECTION('',(0.,0.,-1.));
#19003=DIRECTION('',(0.,1.,0.));
#19004=DIRECTION('',(0.,1.,0.));
#19005=DIRECTION('center_axis',(0.,1.,0.));
#19006=DIRECTION('ref_axis',(1.,0.,0.));
#19007=DIRECTION('center_axis',(0.,1.,0.));
#19008=DIRECTION('ref_axis',(1.,0.,0.));
#19009=DIRECTION('center_axis',(0.,1.,0.));
#19010=DIRECTION('ref_axis',(1.,0.,0.));
#19011=DIRECTION('axis',(0.,0.,1.));
#19012=DIRECTION('refdir',(1.,0.,0.));
#19013=DIRECTION('center_axis',(0.,1.,0.));
#19014=DIRECTION('ref_axis',(0.,0.,1.));
#19015=DIRECTION('center_axis',(0.,-1.,0.));
#19016=DIRECTION('ref_axis',(1.,0.,0.));
#19017=DIRECTION('center_axis',(0.,-1.,0.));
#19018=DIRECTION('ref_axis',(1.,0.,0.));
#19019=DIRECTION('center_axis',(0.,-1.,0.));
#19020=DIRECTION('ref_axis',(1.,0.,0.));
#19021=DIRECTION('',(0.707106781186547,0.707106781186548,8.65956056235493E-17));
#19022=DIRECTION('center_axis',(0.,-1.,0.));
#19023=DIRECTION('ref_axis',(1.,0.,0.));
#19024=DIRECTION('center_axis',(0.,-1.,0.));
#19025=DIRECTION('ref_axis',(1.,0.,0.));
#19026=DIRECTION('',(0.,1.,0.));
#19027=DIRECTION('center_axis',(0.,1.,0.));
#19028=DIRECTION('ref_axis',(1.,0.,0.));
#19029=DIRECTION('center_axis',(0.,-1.,0.));
#19030=DIRECTION('ref_axis',(1.,0.,0.));
#19031=DIRECTION('',(-0.707106781186547,0.707106781186548,-8.65956056235493E-17));
#19032=DIRECTION('center_axis',(0.,-1.,0.));
#19033=DIRECTION('ref_axis',(0.,0.,-1.));
#19034=DIRECTION('center_axis',(0.,-1.,0.));
#19035=DIRECTION('ref_axis',(1.,0.,0.));
#19036=DIRECTION('center_axis',(0.,1.,0.));
#19037=DIRECTION('ref_axis',(1.,0.,0.));
#19038=DIRECTION('center_axis',(0.,1.,0.));
#19039=DIRECTION('ref_axis',(1.,0.,0.));
#19040=DIRECTION('',(-0.447213595499958,0.894427190999916,-5.47678698264203E-17));
#19041=DIRECTION('center_axis',(0.,-1.,0.));
#19042=DIRECTION('ref_axis',(1.,0.,0.));
#19043=DIRECTION('center_axis',(0.,1.,0.));
#19044=DIRECTION('ref_axis',(1.,0.,0.));
#19045=DIRECTION('',(0.,1.,0.));
#19046=DIRECTION('center_axis',(0.,1.,0.));
#19047=DIRECTION('ref_axis',(1.,0.,0.));
#19048=DIRECTION('center_axis',(0.,-1.,0.));
#19049=DIRECTION('ref_axis',(1.,0.,0.));
#19050=DIRECTION('',(-0.707106781186547,0.707106781186548,-8.65956056235493E-17));
#19051=DIRECTION('center_axis',(0.,-1.,0.));
#19052=DIRECTION('ref_axis',(0.,0.,-1.));
#19053=DIRECTION('center_axis',(0.866025403784439,0.,-0.5));
#19054=DIRECTION('ref_axis',(0.5,0.,0.866025403784439));
#19055=DIRECTION('',(-0.5,0.,-0.866025403784439));
#19056=DIRECTION('',(0.,-1.,0.));
#19057=DIRECTION('',(0.5,0.,0.866025403784439));
#19058=DIRECTION('',(0.,-1.,0.));
#19059=DIRECTION('center_axis',(1.60246890531964E-16,0.,-1.));
#19060=DIRECTION('ref_axis',(1.,0.,1.60246890531964E-16));
#19061=DIRECTION('',(-1.,0.,-1.60246890531964E-16));
#19062=DIRECTION('',(0.,-1.,0.));
#19063=DIRECTION('',(1.,0.,1.60246890531964E-16));
#19064=DIRECTION('center_axis',(-0.866025403784439,0.,-0.5));
#19065=DIRECTION('ref_axis',(0.5,0.,-0.866025403784439));
#19066=DIRECTION('',(-0.5,0.,0.866025403784439));
#19067=DIRECTION('',(0.,-1.,0.));
#19068=DIRECTION('',(0.5,0.,-0.866025403784439));
#19069=DIRECTION('center_axis',(-0.866025403784439,0.,0.5));
#19070=DIRECTION('ref_axis',(-0.5,0.,-0.866025403784439));
#19071=DIRECTION('',(0.5,0.,0.866025403784439));
#19072=DIRECTION('',(0.,-1.,0.));
#19073=DIRECTION('',(-0.5,0.,-0.866025403784439));
#19074=DIRECTION('center_axis',(-1.60246890531964E-16,0.,1.));
#19075=DIRECTION('ref_axis',(-1.,0.,-1.60246890531964E-16));
#19076=DIRECTION('',(1.,0.,1.60246890531964E-16));
#19077=DIRECTION('',(0.,-1.,0.));
#19078=DIRECTION('',(-1.,0.,-1.60246890531964E-16));
#19079=DIRECTION('center_axis',(0.866025403784439,0.,0.5));
#19080=DIRECTION('ref_axis',(-0.5,0.,0.866025403784439));
#19081=DIRECTION('',(0.5,0.,-0.866025403784439));
#19082=DIRECTION('',(-0.5,0.,0.866025403784439));
#19083=DIRECTION('center_axis',(0.,1.,0.));
#19084=DIRECTION('ref_axis',(1.,0.,0.));
#19085=DIRECTION('center_axis',(0.,-1.,0.));
#19086=DIRECTION('ref_axis',(0.,0.,-1.));
#19087=DIRECTION('',(0.,0.,1.));
#19088=DIRECTION('',(1.,0.,0.));
#19089=DIRECTION('',(0.,0.,1.));
#19090=DIRECTION('',(1.,0.,0.));
#19091=DIRECTION('',(0.,0.,1.));
#19092=DIRECTION('',(1.,0.,0.));
#19093=DIRECTION('',(0.,0.,1.));
#19094=DIRECTION('',(1.,0.,0.));
#19095=DIRECTION('',(0.,0.,1.));
#19096=DIRECTION('',(1.,0.,0.));
#19097=DIRECTION('',(0.,0.,1.));
#19098=DIRECTION('',(1.,0.,0.));
#19099=DIRECTION('',(0.,0.,1.));
#19100=DIRECTION('',(1.,0.,0.));
#19101=DIRECTION('',(0.,0.,1.));
#19102=DIRECTION('',(1.,0.,0.));
#19103=DIRECTION('',(0.,0.,1.));
#19104=DIRECTION('',(1.,0.,0.));
#19105=DIRECTION('',(0.,0.,1.));
#19106=DIRECTION('',(1.,0.,0.));
#19107=DIRECTION('',(0.,0.,1.));
#19108=DIRECTION('',(1.,0.,0.));
#19109=DIRECTION('',(0.,0.,1.));
#19110=DIRECTION('',(1.,0.,0.));
#19111=DIRECTION('',(0.,0.,1.));
#19112=DIRECTION('',(1.,0.,0.));
#19113=DIRECTION('',(0.,0.,1.));
#19114=DIRECTION('',(1.,0.,0.));
#19115=DIRECTION('',(0.,0.,1.));
#19116=DIRECTION('',(1.,0.,0.));
#19117=DIRECTION('',(0.,0.,1.));
#19118=DIRECTION('',(1.,0.,0.));
#19119=DIRECTION('',(0.,0.,1.));
#19120=DIRECTION('',(1.,0.,0.));
#19121=DIRECTION('',(0.,-1.,2.22044604925031E-16));
#19122=DIRECTION('',(1.,0.,0.));
#19123=DIRECTION('',(0.,-1.,2.22044604925031E-16));
#19124=DIRECTION('',(1.,0.,0.));
#19125=DIRECTION('',(0.,-1.22464679914735E-16,-1.));
#19126=DIRECTION('',(1.,0.,0.));
#19127=DIRECTION('',(0.,1.,2.22044604925031E-16));
#19128=DIRECTION('',(1.,0.,0.));
#19129=DIRECTION('',(0.,1.,2.22044604925031E-16));
#19130=DIRECTION('',(1.,0.,0.));
#19131=DIRECTION('',(0.,0.,1.));
#19132=DIRECTION('',(1.,0.,0.));
#19133=DIRECTION('',(0.,-1.,2.22044604925031E-16));
#19134=DIRECTION('',(1.,0.,0.));
#19135=DIRECTION('',(0.,-1.,2.22044604925031E-16));
#19136=DIRECTION('',(1.,0.,0.));
#19137=DIRECTION('',(0.,-1.22464679914735E-16,-1.));
#19138=DIRECTION('',(1.,0.,0.));
#19139=DIRECTION('',(0.,1.,2.22044604925031E-16));
#19140=DIRECTION('',(1.,0.,0.));
#19141=DIRECTION('',(0.,1.,2.22044604925031E-16));
#19142=DIRECTION('',(1.,0.,0.));
#19143=DIRECTION('',(0.,0.,1.));
#19144=DIRECTION('',(1.,0.,0.));
#19145=DIRECTION('',(0.,-1.,2.22044604925031E-16));
#19146=DIRECTION('',(1.,0.,0.));
#19147=DIRECTION('',(0.,-1.,2.22044604925031E-16));
#19148=DIRECTION('',(1.,0.,0.));
#19149=DIRECTION('',(0.,-1.22464679914735E-16,-1.));
#19150=DIRECTION('',(1.,0.,0.));
#19151=DIRECTION('',(0.,1.,2.22044604925031E-16));
#19152=DIRECTION('',(1.,0.,0.));
#19153=DIRECTION('',(0.,1.,2.22044604925031E-16));
#19154=DIRECTION('',(1.,0.,0.));
#19155=DIRECTION('',(0.,0.,1.));
#19156=DIRECTION('',(1.,0.,0.));
#19157=DIRECTION('',(0.,-1.,2.22044604925031E-16));
#19158=DIRECTION('',(1.,0.,0.));
#19159=DIRECTION('',(0.,-1.,2.22044604925031E-16));
#19160=DIRECTION('',(1.,0.,0.));
#19161=DIRECTION('',(0.,-1.22464679914735E-16,-1.));
#19162=DIRECTION('',(1.,0.,0.));
#19163=DIRECTION('',(0.,1.,2.22044604925031E-16));
#19164=DIRECTION('',(1.,0.,0.));
#19165=DIRECTION('',(0.,1.,2.22044604925031E-16));
#19166=DIRECTION('',(1.,0.,0.));
#19167=DIRECTION('',(0.,0.,1.));
#19168=DIRECTION('',(1.,0.,0.));
#19169=DIRECTION('',(0.,-1.,2.22044604925031E-16));
#19170=DIRECTION('',(1.,0.,0.));
#19171=DIRECTION('',(0.,-1.,2.22044604925031E-16));
#19172=DIRECTION('',(1.,0.,0.));
#19173=DIRECTION('',(0.,-1.,2.22044604925031E-16));
#19174=DIRECTION('',(1.,0.,0.));
#19175=DIRECTION('',(0.,-1.,2.22044604925031E-16));
#19176=DIRECTION('',(1.,0.,0.));
#19177=DIRECTION('',(0.,-1.,2.22044604925031E-16));
#19178=DIRECTION('',(1.,0.,0.));
#19179=DIRECTION('',(0.,-1.,2.22044604925031E-16));
#19180=DIRECTION('',(1.,0.,0.));
#19181=DIRECTION('',(0.,-1.,2.22044604925031E-16));
#19182=DIRECTION('',(1.,0.,0.));
#19183=DIRECTION('',(0.,-1.,2.22044604925031E-16));
#19184=DIRECTION('',(1.,0.,0.));
#19185=DIRECTION('',(0.,-1.,2.22044604925031E-16));
#19186=DIRECTION('',(1.,0.,0.));
#19187=DIRECTION('',(0.,-1.,2.22044604925031E-16));
#19188=DIRECTION('',(1.,0.,0.));
#19189=DIRECTION('',(0.,0.,1.));
#19190=DIRECTION('',(1.,0.,0.));
#19191=DIRECTION('',(0.,0.,1.));
#19192=DIRECTION('',(-1.,1.22464679914735E-16,0.));
#19193=DIRECTION('',(0.,0.,1.));
#19194=DIRECTION('',(-1.,1.22464679914735E-16,0.));
#19195=DIRECTION('',(0.,0.,1.));
#19196=DIRECTION('',(-1.,1.22464679914735E-16,0.));
#19197=DIRECTION('',(0.,0.,1.));
#19198=DIRECTION('',(-1.,1.22464679914735E-16,0.));
#19199=DIRECTION('',(0.,0.,1.));
#19200=DIRECTION('',(1.,0.,0.));
#19201=DIRECTION('',(0.,0.,1.));
#19202=DIRECTION('',(1.,0.,0.));
#19203=DIRECTION('',(0.,0.,1.));
#19204=DIRECTION('',(1.,0.,0.));
#19205=DIRECTION('',(0.,0.,1.));
#19206=DIRECTION('',(1.,0.,0.));
#19207=DIRECTION('',(0.,-1.,2.22044604925031E-16));
#19208=DIRECTION('',(1.,0.,0.));
#19209=DIRECTION('',(0.,-1.,2.22044604925031E-16));
#19210=DIRECTION('',(1.,0.,0.));
#19211=DIRECTION('',(0.,0.,1.));
#19212=DIRECTION('',(1.,0.,0.));
#19213=DIRECTION('',(0.,0.,1.));
#19214=DIRECTION('',(-1.,1.22464679914735E-16,0.));
#19215=DIRECTION('',(0.,0.,1.));
#19216=DIRECTION('',(-1.,1.22464679914735E-16,0.));
#19217=DIRECTION('',(0.,0.,1.));
#19218=DIRECTION('',(-1.,1.22464679914735E-16,0.));
#19219=DIRECTION('',(0.,0.,1.));
#19220=DIRECTION('',(-1.,1.22464679914735E-16,0.));
#19221=DIRECTION('',(0.,0.,1.));
#19222=DIRECTION('',(1.,0.,0.));
#19223=DIRECTION('',(0.,0.,1.));
#19224=DIRECTION('',(1.,0.,0.));
#19225=DIRECTION('',(0.,0.,1.));
#19226=DIRECTION('',(1.,0.,0.));
#19227=DIRECTION('',(0.,0.,1.));
#19228=DIRECTION('',(1.,0.,0.));
#19229=DIRECTION('',(0.,0.,1.));
#19230=DIRECTION('',(1.,0.,0.));
#19231=DIRECTION('',(0.,0.,1.));
#19232=DIRECTION('',(1.,0.,0.));
#19233=DIRECTION('',(0.,0.,1.));
#19234=DIRECTION('',(1.,0.,0.));
#19235=DIRECTION('',(0.,-1.,2.22044604925031E-16));
#19236=DIRECTION('',(1.,0.,0.));
#19237=DIRECTION('',(0.,-1.,2.22044604925031E-16));
#19238=DIRECTION('',(1.,0.,0.));
#19239=DIRECTION('',(0.,-1.,2.22044604925031E-16));
#19240=DIRECTION('',(1.,0.,0.));
#19241=DIRECTION('',(0.,-1.,2.22044604925031E-16));
#19242=DIRECTION('',(1.,0.,0.));
#19243=DIRECTION('',(0.,1.,2.22044604925031E-16));
#19244=DIRECTION('',(1.,0.,0.));
#19245=DIRECTION('',(0.,1.,2.22044604925031E-16));
#19246=DIRECTION('',(1.,0.,0.));
#19247=DIRECTION('',(0.,1.,2.22044604925031E-16));
#19248=DIRECTION('',(1.,0.,0.));
#19249=DIRECTION('',(0.,1.,2.22044604925031E-16));
#19250=DIRECTION('',(1.,0.,0.));
#19251=DIRECTION('axis',(0.,0.,1.));
#19252=DIRECTION('refdir',(1.,0.,0.));
#19253=DIRECTION('center_axis',(1.,0.,0.));
#19254=DIRECTION('ref_axis',(0.,0.,-1.));
#19255=DIRECTION('',(0.,0.707106781186547,-0.707106781186548));
#19256=DIRECTION('',(0.,1.,0.));
#19257=DIRECTION('',(0.,0.707106781186547,0.707106781186548));
#19258=DIRECTION('',(0.,0.,1.));
#19259=DIRECTION('',(0.,-0.707106781186548,0.707106781186548));
#19260=DIRECTION('',(0.,-1.,0.));
#19261=DIRECTION('',(0.,-0.707106781186548,-0.707106781186548));
#19262=DIRECTION('',(0.,0.,-1.));
#19263=DIRECTION('center_axis',(0.,-0.707106781186548,-0.707106781186548));
#19264=DIRECTION('ref_axis',(-1.,0.,0.));
#19265=DIRECTION('',(-1.,0.,0.));
#19266=DIRECTION('',(0.,0.707106781186548,-0.707106781186548));
#19267=DIRECTION('',(1.,0.,0.));
#19268=DIRECTION('center_axis',(0.,-1.,0.));
#19269=DIRECTION('ref_axis',(1.,0.,0.));
#19270=DIRECTION('',(1.,0.,0.));
#19271=DIRECTION('',(0.,0.,-1.));
#19272=DIRECTION('center_axis',(0.,-0.707106781186548,0.707106781186547));
#19273=DIRECTION('ref_axis',(1.,0.,0.));
#19274=DIRECTION('',(-1.,0.,0.));
#19275=DIRECTION('',(0.,-0.707106781186547,-0.707106781186548));
#19276=DIRECTION('center_axis',(0.,0.,1.));
#19277=DIRECTION('ref_axis',(1.,0.,0.));
#19278=DIRECTION('',(1.,0.,0.));
#19279=DIRECTION('',(0.,-1.,0.));
#19280=DIRECTION('center_axis',(1.,0.,0.));
#19281=DIRECTION('ref_axis',(0.,0.,-1.));
#19282=DIRECTION('',(0.,-0.707106781186547,0.707106781186548));
#19283=DIRECTION('',(0.,0.,1.));
#19284=DIRECTION('',(0.,0.707106781186548,0.707106781186548));
#19285=DIRECTION('',(0.,1.,0.));
#19286=DIRECTION('center_axis',(0.,0.707106781186548,0.707106781186547));
#19287=DIRECTION('ref_axis',(1.,0.,0.));
#19288=DIRECTION('',(-1.,0.,0.));
#19289=DIRECTION('center_axis',(0.,1.,0.));
#19290=DIRECTION('ref_axis',(-1.,0.,0.));
#19291=DIRECTION('',(1.,0.,0.));
#19292=DIRECTION('center_axis',(0.,0.707106781186548,-0.707106781186548));
#19293=DIRECTION('ref_axis',(-1.,0.,0.));
#19294=DIRECTION('',(-1.,0.,0.));
#19295=DIRECTION('center_axis',(0.,0.,1.));
#19296=DIRECTION('ref_axis',(1.,0.,0.));
#19297=DIRECTION('axis',(0.,0.,1.));
#19298=DIRECTION('refdir',(1.,0.,0.));
#19299=DIRECTION('center_axis',(0.,1.,0.));
#19300=DIRECTION('ref_axis',(1.,0.,0.));
#19301=DIRECTION('center_axis',(0.,-1.,0.));
#19302=DIRECTION('ref_axis',(1.,0.,0.));
#19303=DIRECTION('',(0.,-1.,0.));
#19304=DIRECTION('center_axis',(0.,-1.,0.));
#19305=DIRECTION('ref_axis',(1.,0.,0.));
#19306=DIRECTION('center_axis',(0.,1.,0.));
#19307=DIRECTION('ref_axis',(1.,0.,0.));
#19308=DIRECTION('center_axis',(0.,1.,0.));
#19309=DIRECTION('ref_axis',(1.,0.,0.));
#19310=DIRECTION('',(0.,-1.,0.));
#19311=DIRECTION('center_axis',(0.,1.,0.));
#19312=DIRECTION('ref_axis',(1.,0.,0.));
#19313=DIRECTION('center_axis',(0.,1.,0.));
#19314=DIRECTION('ref_axis',(1.,0.,0.));
#19315=DIRECTION('center_axis',(0.,1.,0.));
#19316=DIRECTION('ref_axis',(1.,0.,0.));
#19317=DIRECTION('axis',(0.,0.,1.));
#19318=DIRECTION('refdir',(1.,0.,0.));
#19319=DIRECTION('center_axis',(0.,1.,0.));
#19320=DIRECTION('ref_axis',(0.,0.,1.));
#19321=DIRECTION('center_axis',(0.,-1.,0.));
#19322=DIRECTION('ref_axis',(1.,0.,0.));
#19323=DIRECTION('center_axis',(0.,-1.,0.));
#19324=DIRECTION('ref_axis',(1.,0.,0.));
#19325=DIRECTION('center_axis',(0.,-1.,0.));
#19326=DIRECTION('ref_axis',(1.,0.,0.));
#19327=DIRECTION('',(0.707106781186548,0.707106781186547,8.65956056235494E-17));
#19328=DIRECTION('center_axis',(0.,-1.,0.));
#19329=DIRECTION('ref_axis',(1.,0.,0.));
#19330=DIRECTION('center_axis',(0.,-1.,0.));
#19331=DIRECTION('ref_axis',(1.,0.,0.));
#19332=DIRECTION('',(0.,1.,0.));
#19333=DIRECTION('center_axis',(0.,1.,0.));
#19334=DIRECTION('ref_axis',(1.,0.,0.));
#19335=DIRECTION('center_axis',(0.,-1.,0.));
#19336=DIRECTION('ref_axis',(1.,0.,0.));
#19337=DIRECTION('',(-0.707106781186547,0.707106781186548,-8.65956056235493E-17));
#19338=DIRECTION('center_axis',(0.,-1.,0.));
#19339=DIRECTION('ref_axis',(0.,0.,-1.));
#19340=DIRECTION('center_axis',(0.,-1.,0.));
#19341=DIRECTION('ref_axis',(1.,0.,0.));
#19342=DIRECTION('center_axis',(0.,1.,0.));
#19343=DIRECTION('ref_axis',(1.,0.,0.));
#19344=DIRECTION('center_axis',(0.,1.,0.));
#19345=DIRECTION('ref_axis',(1.,0.,0.));
#19346=DIRECTION('',(-0.447213595499958,0.894427190999916,-5.47678698264203E-17));
#19347=DIRECTION('center_axis',(0.,-1.,0.));
#19348=DIRECTION('ref_axis',(1.,0.,0.));
#19349=DIRECTION('center_axis',(0.,1.,0.));
#19350=DIRECTION('ref_axis',(1.,0.,0.));
#19351=DIRECTION('',(0.,1.,0.));
#19352=DIRECTION('center_axis',(0.,1.,0.));
#19353=DIRECTION('ref_axis',(1.,0.,0.));
#19354=DIRECTION('center_axis',(0.,-1.,0.));
#19355=DIRECTION('ref_axis',(1.,0.,0.));
#19356=DIRECTION('',(-0.707106781186547,0.707106781186548,-8.65956056235493E-17));
#19357=DIRECTION('center_axis',(0.,-1.,0.));
#19358=DIRECTION('ref_axis',(0.,0.,-1.));
#19359=DIRECTION('center_axis',(0.866025403784439,0.,-0.5));
#19360=DIRECTION('ref_axis',(0.5,0.,0.866025403784439));
#19361=DIRECTION('',(-0.5,0.,-0.866025403784439));
#19362=DIRECTION('',(0.,-1.,0.));
#19363=DIRECTION('',(0.5,0.,0.866025403784439));
#19364=DIRECTION('',(0.,-1.,0.));
#19365=DIRECTION('center_axis',(1.92296268638356E-16,0.,-1.));
#19366=DIRECTION('ref_axis',(1.,0.,1.92296268638356E-16));
#19367=DIRECTION('',(-1.,0.,-1.92296268638356E-16));
#19368=DIRECTION('',(0.,-1.,0.));
#19369=DIRECTION('',(1.,0.,1.92296268638356E-16));
#19370=DIRECTION('center_axis',(-0.866025403784439,0.,-0.5));
#19371=DIRECTION('ref_axis',(0.5,0.,-0.866025403784439));
#19372=DIRECTION('',(-0.5,0.,0.866025403784438));
#19373=DIRECTION('',(0.,-1.,0.));
#19374=DIRECTION('',(0.5,0.,-0.866025403784438));
#19375=DIRECTION('center_axis',(-0.866025403784439,0.,0.5));
#19376=DIRECTION('ref_axis',(-0.5,0.,-0.866025403784439));
#19377=DIRECTION('',(0.5,0.,0.866025403784439));
#19378=DIRECTION('',(0.,-1.,0.));
#19379=DIRECTION('',(-0.5,0.,-0.866025403784439));
#19380=DIRECTION('center_axis',(-1.92296268638356E-16,0.,1.));
#19381=DIRECTION('ref_axis',(-1.,0.,-1.92296268638356E-16));
#19382=DIRECTION('',(1.,0.,1.92296268638356E-16));
#19383=DIRECTION('',(0.,-1.,0.));
#19384=DIRECTION('',(-1.,0.,-1.92296268638356E-16));
#19385=DIRECTION('center_axis',(0.866025403784439,0.,0.5));
#19386=DIRECTION('ref_axis',(-0.5,0.,0.866025403784439));
#19387=DIRECTION('',(0.5,0.,-0.866025403784439));
#19388=DIRECTION('',(-0.5,0.,0.866025403784439));
#19389=DIRECTION('center_axis',(0.,1.,0.));
#19390=DIRECTION('ref_axis',(1.,0.,0.));
#19391=DIRECTION('center_axis',(0.,-1.,0.));
#19392=DIRECTION('ref_axis',(0.,0.,-1.));
#19393=DIRECTION('',(0.,0.,1.));
#19394=DIRECTION('',(1.,0.,0.));
#19395=DIRECTION('',(0.,0.,1.));
#19396=DIRECTION('',(1.,0.,0.));
#19397=DIRECTION('',(0.,0.,1.));
#19398=DIRECTION('',(1.,0.,0.));
#19399=DIRECTION('',(0.,0.,1.));
#19400=DIRECTION('',(1.,0.,0.));
#19401=DIRECTION('',(0.,0.,1.));
#19402=DIRECTION('',(1.,0.,0.));
#19403=DIRECTION('',(0.,0.,1.));
#19404=DIRECTION('',(1.,0.,0.));
#19405=DIRECTION('',(0.,0.,1.));
#19406=DIRECTION('',(1.,0.,0.));
#19407=DIRECTION('',(0.,0.,1.));
#19408=DIRECTION('',(1.,0.,0.));
#19409=DIRECTION('',(0.,0.,1.));
#19410=DIRECTION('',(1.,0.,0.));
#19411=DIRECTION('',(0.,0.,1.));
#19412=DIRECTION('',(1.,0.,0.));
#19413=DIRECTION('',(8.65956056235493E-17,-8.65956056235493E-17,-1.));
#19414=DIRECTION('',(2.22044604925031E-16,1.,-8.65956056235494E-17));
#19415=DIRECTION('',(0.,0.,1.));
#19416=DIRECTION('',(-1.,1.22464679914735E-16,0.));
#19417=DIRECTION('',(0.,0.,1.));
#19418=DIRECTION('',(1.,0.,0.));
#19419=DIRECTION('',(8.65956056235493E-17,-8.65956056235493E-17,-1.));
#19420=DIRECTION('',(2.22044604925031E-16,1.,-8.65956056235494E-17));
#19421=DIRECTION('',(0.,0.,1.));
#19422=DIRECTION('',(1.,0.,0.));
#19423=DIRECTION('',(0.,0.,1.));
#19424=DIRECTION('',(1.,0.,0.));
#19425=DIRECTION('axis',(0.,0.,1.));
#19426=DIRECTION('refdir',(1.,0.,0.));
#19427=DIRECTION('axis',(0.,0.,1.));
#19428=DIRECTION('refdir',(1.,0.,0.));
#19429=DIRECTION('center_axis',(0.,1.,0.));
#19430=DIRECTION('ref_axis',(1.,0.,0.));
#19431=DIRECTION('center_axis',(0.,-1.,0.));
#19432=DIRECTION('ref_axis',(1.,0.,0.));
#19433=DIRECTION('',(0.,-1.,0.));
#19434=DIRECTION('center_axis',(0.,-1.,0.));
#19435=DIRECTION('ref_axis',(1.,0.,0.));
#19436=DIRECTION('center_axis',(0.,1.,0.));
#19437=DIRECTION('ref_axis',(1.,0.,0.));
#19438=DIRECTION('center_axis',(0.,1.,0.));
#19439=DIRECTION('ref_axis',(1.,0.,0.));
#19440=DIRECTION('',(0.,-1.,0.));
#19441=DIRECTION('center_axis',(0.,1.,0.));
#19442=DIRECTION('ref_axis',(1.,0.,0.));
#19443=DIRECTION('center_axis',(0.,1.,0.));
#19444=DIRECTION('ref_axis',(1.,0.,0.));
#19445=DIRECTION('center_axis',(0.,1.,0.));
#19446=DIRECTION('ref_axis',(1.,0.,0.));
#19447=DIRECTION('',(0.,0.,1.));
#19448=DIRECTION('',(1.,0.,0.));
#19449=DIRECTION('',(0.,0.,1.));
#19450=DIRECTION('',(1.,0.,0.));
#19451=DIRECTION('',(0.,0.,1.));
#19452=DIRECTION('',(1.,0.,0.));
#19453=DIRECTION('',(0.,0.,1.));
#19454=DIRECTION('',(1.,0.,0.));
#19455=DIRECTION('',(0.,0.,1.));
#19456=DIRECTION('',(1.,0.,0.));
#19457=CARTESIAN_POINT('',(0.,0.,0.));
#19458=CARTESIAN_POINT('',(0.,0.,0.));
#19459=CARTESIAN_POINT('',(0.,0.,0.));
#19460=CARTESIAN_POINT('Origin',(19.5,4.,-0.1));
#19461=CARTESIAN_POINT('',(19.225,4.,0.));
#19462=CARTESIAN_POINT('Origin',(19.5,4.,0.));
#19463=CARTESIAN_POINT('',(19.225,4.,1.));
#19464=CARTESIAN_POINT('',(19.225,4.,-0.1));
#19465=CARTESIAN_POINT('Origin',(19.5,4.,1.));
#19466=CARTESIAN_POINT('Origin',(19.5,-4.,-0.1));
#19467=CARTESIAN_POINT('',(19.225,-4.,0.));
#19468=CARTESIAN_POINT('Origin',(19.5,-4.,0.));
#19469=CARTESIAN_POINT('',(19.225,-4.,1.));
#19470=CARTESIAN_POINT('',(19.225,-4.,-0.1));
#19471=CARTESIAN_POINT('Origin',(19.5,-4.,1.));
#19472=CARTESIAN_POINT('Origin',(2.5,4.,-0.1));
#19473=CARTESIAN_POINT('',(2.225,4.,0.));
#19474=CARTESIAN_POINT('Origin',(2.5,4.,0.));
#19475=CARTESIAN_POINT('',(2.225,4.,1.));
#19476=CARTESIAN_POINT('',(2.225,4.,-0.1));
#19477=CARTESIAN_POINT('Origin',(2.5,4.,1.));
#19478=CARTESIAN_POINT('Origin',(2.5,-4.,-0.1));
#19479=CARTESIAN_POINT('',(2.225,-4.,0.));
#19480=CARTESIAN_POINT('Origin',(2.5,-4.,0.));
#19481=CARTESIAN_POINT('',(2.225,-4.,1.));
#19482=CARTESIAN_POINT('',(2.225,-4.,-0.1));
#19483=CARTESIAN_POINT('Origin',(2.5,-4.,1.));
#19484=CARTESIAN_POINT('Origin',(28.,7.5,0.));
#19485=CARTESIAN_POINT('',(28.,7.5,0.));
#19486=CARTESIAN_POINT('',(-6.,7.5,0.));
#19487=CARTESIAN_POINT('',(28.,7.5,0.));
#19488=CARTESIAN_POINT('',(-6.,7.5,1.));
#19489=CARTESIAN_POINT('',(-6.,7.5,0.));
#19490=CARTESIAN_POINT('',(28.,7.5,1.));
#19491=CARTESIAN_POINT('',(28.,7.5,1.));
#19492=CARTESIAN_POINT('',(28.,7.5,0.));
#19493=CARTESIAN_POINT('Origin',(28.,-7.5,0.));
#19494=CARTESIAN_POINT('',(28.,-7.5,0.));
#19495=CARTESIAN_POINT('',(28.,-7.5,0.));
#19496=CARTESIAN_POINT('',(28.,-7.5,1.));
#19497=CARTESIAN_POINT('',(28.,-7.5,1.));
#19498=CARTESIAN_POINT('',(28.,-7.5,0.));
#19499=CARTESIAN_POINT('Origin',(-6.,-7.5,0.));
#19500=CARTESIAN_POINT('',(-6.,-7.5,0.));
#19501=CARTESIAN_POINT('',(-6.,-7.5,0.));
#19502=CARTESIAN_POINT('',(-6.,-7.5,1.));
#19503=CARTESIAN_POINT('',(-6.,-7.5,1.));
#19504=CARTESIAN_POINT('',(-6.,-7.5,0.));
#19505=CARTESIAN_POINT('Origin',(-6.,7.5,0.));
#19506=CARTESIAN_POINT('',(-6.,7.5,0.));
#19507=CARTESIAN_POINT('',(-6.,7.5,1.));
#19508=CARTESIAN_POINT('Origin',(11.,0.,1.));
#19509=CARTESIAN_POINT('Origin',(11.,0.,0.));
#19510=CARTESIAN_POINT('',(0.,0.,0.));
#19511=CARTESIAN_POINT('Origin',(-4.,7.5,-1.));
#19512=CARTESIAN_POINT('',(-4.,7.5,-1.));
#19513=CARTESIAN_POINT('',(-6.,7.5,-1.));
#19514=CARTESIAN_POINT('',(-4.,7.5,-1.));
#19515=CARTESIAN_POINT('',(-6.,7.5,0.));
#19516=CARTESIAN_POINT('',(-6.,7.5,-1.));
#19517=CARTESIAN_POINT('',(-4.,7.5,0.));
#19518=CARTESIAN_POINT('',(-4.,7.5,0.));
#19519=CARTESIAN_POINT('',(-4.,7.5,-1.));
#19520=CARTESIAN_POINT('Origin',(-4.,-7.5,-1.));
#19521=CARTESIAN_POINT('',(-4.,-7.5,-1.));
#19522=CARTESIAN_POINT('',(-4.,-7.5,-1.));
#19523=CARTESIAN_POINT('',(-4.,-7.5,0.));
#19524=CARTESIAN_POINT('',(-4.,-7.5,0.));
#19525=CARTESIAN_POINT('',(-4.,-7.5,-1.));
#19526=CARTESIAN_POINT('Origin',(-6.,-7.5,-1.));
#19527=CARTESIAN_POINT('',(-6.,-7.5,-1.));
#19528=CARTESIAN_POINT('',(-6.,-7.5,-1.));
#19529=CARTESIAN_POINT('',(-6.,-7.5,0.));
#19530=CARTESIAN_POINT('',(-6.,-7.5,0.));
#19531=CARTESIAN_POINT('',(-6.,-7.5,-1.));
#19532=CARTESIAN_POINT('Origin',(-6.,7.5,-1.));
#19533=CARTESIAN_POINT('',(-6.,7.5,-1.));
#19534=CARTESIAN_POINT('',(-6.,7.5,0.));
#19535=CARTESIAN_POINT('Origin',(-5.,0.,0.));
#19536=CARTESIAN_POINT('Origin',(-5.,0.,-1.));
#19537=CARTESIAN_POINT('',(0.,0.,0.));
#19538=CARTESIAN_POINT('Origin',(28.,7.5,-1.));
#19539=CARTESIAN_POINT('',(28.,7.5,-1.));
#19540=CARTESIAN_POINT('',(26.,7.5,-1.));
#19541=CARTESIAN_POINT('',(28.,7.5,-1.));
#19542=CARTESIAN_POINT('',(26.,7.5,0.));
#19543=CARTESIAN_POINT('',(26.,7.5,-1.));
#19544=CARTESIAN_POINT('',(28.,7.5,0.));
#19545=CARTESIAN_POINT('',(28.,7.5,0.));
#19546=CARTESIAN_POINT('',(28.,7.5,-1.));
#19547=CARTESIAN_POINT('Origin',(28.,-7.5,-1.));
#19548=CARTESIAN_POINT('',(28.,-7.5,-1.));
#19549=CARTESIAN_POINT('',(28.,-7.5,-1.));
#19550=CARTESIAN_POINT('',(28.,-7.5,0.));
#19551=CARTESIAN_POINT('',(28.,-7.5,0.));
#19552=CARTESIAN_POINT('',(28.,-7.5,-1.));
#19553=CARTESIAN_POINT('Origin',(26.,-7.5,-1.));
#19554=CARTESIAN_POINT('',(26.,-7.5,-1.));
#19555=CARTESIAN_POINT('',(26.,-7.5,-1.));
#19556=CARTESIAN_POINT('',(26.,-7.5,0.));
#19557=CARTESIAN_POINT('',(26.,-7.5,0.));
#19558=CARTESIAN_POINT('',(26.,-7.5,-1.));
#19559=CARTESIAN_POINT('Origin',(26.,7.5,-1.));
#19560=CARTESIAN_POINT('',(26.,7.5,-1.));
#19561=CARTESIAN_POINT('',(26.,7.5,0.));
#19562=CARTESIAN_POINT('Origin',(27.,0.,0.));
#19563=CARTESIAN_POINT('Origin',(27.,0.,-1.));
#19564=CARTESIAN_POINT('',(0.,0.,0.));
#19565=CARTESIAN_POINT('Origin',(8.,4.2,2.9));
#19566=CARTESIAN_POINT('',(7.835,4.2,3.));
#19567=CARTESIAN_POINT('Origin',(8.,4.2,3.));
#19568=CARTESIAN_POINT('',(7.835,4.2,3.8));
#19569=CARTESIAN_POINT('',(7.835,4.2,2.9));
#19570=CARTESIAN_POINT('Origin',(8.,4.2,3.8));
#19571=CARTESIAN_POINT('Origin',(14.,4.2,2.9));
#19572=CARTESIAN_POINT('',(13.835,4.2,3.));
#19573=CARTESIAN_POINT('Origin',(14.,4.2,3.));
#19574=CARTESIAN_POINT('',(13.835,4.2,3.8));
#19575=CARTESIAN_POINT('',(13.835,4.2,2.9));
#19576=CARTESIAN_POINT('Origin',(14.,4.2,3.8));
#19577=CARTESIAN_POINT('Origin',(8.,-4.2,2.9));
#19578=CARTESIAN_POINT('',(7.835,-4.2,3.));
#19579=CARTESIAN_POINT('Origin',(8.,-4.2,3.));
#19580=CARTESIAN_POINT('',(7.835,-4.2,3.8));
#19581=CARTESIAN_POINT('',(7.835,-4.2,2.9));
#19582=CARTESIAN_POINT('Origin',(8.,-4.2,3.8));
#19583=CARTESIAN_POINT('Origin',(14.,-4.2,2.9));
#19584=CARTESIAN_POINT('',(13.835,-4.2,3.));
#19585=CARTESIAN_POINT('Origin',(14.,-4.2,3.));
#19586=CARTESIAN_POINT('',(13.835,-4.2,3.8));
#19587=CARTESIAN_POINT('',(13.835,-4.2,2.9));
#19588=CARTESIAN_POINT('Origin',(14.,-4.2,3.8));
#19589=CARTESIAN_POINT('Origin',(26.2,-1.8,2.9));
#19590=CARTESIAN_POINT('',(25.99,-1.8,3.));
#19591=CARTESIAN_POINT('Origin',(26.2,-1.8,3.));
#19592=CARTESIAN_POINT('',(25.99,-1.8,3.8));
#19593=CARTESIAN_POINT('',(25.99,-1.8,2.9));
#19594=CARTESIAN_POINT('Origin',(26.2,-1.8,3.8));
#19595=CARTESIAN_POINT('Origin',(26.2,1.8,2.9));
#19596=CARTESIAN_POINT('',(25.99,1.8,3.));
#19597=CARTESIAN_POINT('Origin',(26.2,1.8,3.));
#19598=CARTESIAN_POINT('',(25.99,1.8,3.8));
#19599=CARTESIAN_POINT('',(25.99,1.8,2.9));
#19600=CARTESIAN_POINT('Origin',(26.2,1.8,3.8));
#19601=CARTESIAN_POINT('Origin',(-4.2,-1.8,2.9));
#19602=CARTESIAN_POINT('',(-4.41,-1.8,3.));
#19603=CARTESIAN_POINT('Origin',(-4.2,-1.8,3.));
#19604=CARTESIAN_POINT('',(-4.41,-1.8,3.8));
#19605=CARTESIAN_POINT('',(-4.41,-1.8,2.9));
#19606=CARTESIAN_POINT('Origin',(-4.2,-1.8,3.8));
#19607=CARTESIAN_POINT('Origin',(-4.2,1.8,2.9));
#19608=CARTESIAN_POINT('',(-4.41,1.8,3.));
#19609=CARTESIAN_POINT('Origin',(-4.2,1.8,3.));
#19610=CARTESIAN_POINT('',(-4.41,1.8,3.8));
#19611=CARTESIAN_POINT('',(-4.41,1.8,2.9));
#19612=CARTESIAN_POINT('Origin',(-4.2,1.8,3.8));
#19613=CARTESIAN_POINT('Origin',(14.,0.,2.9));
#19614=CARTESIAN_POINT('',(13.835,-2.02066721859312E-17,3.));
#19615=CARTESIAN_POINT('Origin',(14.,0.,3.));
#19616=CARTESIAN_POINT('',(13.835,2.02066721859312E-17,3.8));
#19617=CARTESIAN_POINT('',(13.835,-2.02066721859312E-17,2.9));
#19618=CARTESIAN_POINT('Origin',(14.,0.,3.8));
#19619=CARTESIAN_POINT('Origin',(8.,0.,2.9));
#19620=CARTESIAN_POINT('',(7.835,-2.02066721859312E-17,3.));
#19621=CARTESIAN_POINT('Origin',(8.,0.,3.));
#19622=CARTESIAN_POINT('',(7.835,2.02066721859312E-17,3.8));
#19623=CARTESIAN_POINT('',(7.835,-2.02066721859312E-17,2.9));
#19624=CARTESIAN_POINT('Origin',(8.,0.,3.8));
#19625=CARTESIAN_POINT('Origin',(2.,0.,2.9));
#19626=CARTESIAN_POINT('',(1.835,-2.02066721859313E-17,3.));
#19627=CARTESIAN_POINT('Origin',(2.,0.,3.));
#19628=CARTESIAN_POINT('',(1.835,2.02066721859313E-17,3.8));
#19629=CARTESIAN_POINT('',(1.835,-2.02066721859313E-17,2.9));
#19630=CARTESIAN_POINT('Origin',(2.,0.,3.8));
#19631=CARTESIAN_POINT('Origin',(20.,0.,2.9));
#19632=CARTESIAN_POINT('',(19.835,-2.02066721859312E-17,3.));
#19633=CARTESIAN_POINT('Origin',(20.,0.,3.));
#19634=CARTESIAN_POINT('',(19.835,2.02066721859312E-17,3.8));
#19635=CARTESIAN_POINT('',(19.835,-2.02066721859312E-17,2.9));
#19636=CARTESIAN_POINT('Origin',(20.,0.,3.8));
#19637=CARTESIAN_POINT('Origin',(19.5,4.,2.9));
#19638=CARTESIAN_POINT('',(19.225,4.,3.));
#19639=CARTESIAN_POINT('Origin',(19.5,4.,3.));
#19640=CARTESIAN_POINT('',(19.225,4.,3.8));
#19641=CARTESIAN_POINT('',(19.225,4.,2.9));
#19642=CARTESIAN_POINT('Origin',(19.5,4.,3.8));
#19643=CARTESIAN_POINT('Origin',(19.5,-4.,2.9));
#19644=CARTESIAN_POINT('',(19.225,-4.,3.));
#19645=CARTESIAN_POINT('Origin',(19.5,-4.,3.));
#19646=CARTESIAN_POINT('',(19.225,-4.,3.8));
#19647=CARTESIAN_POINT('',(19.225,-4.,2.9));
#19648=CARTESIAN_POINT('Origin',(19.5,-4.,3.8));
#19649=CARTESIAN_POINT('Origin',(2.5,4.,2.9));
#19650=CARTESIAN_POINT('',(2.225,4.,3.));
#19651=CARTESIAN_POINT('Origin',(2.5,4.,3.));
#19652=CARTESIAN_POINT('',(2.225,4.,3.8));
#19653=CARTESIAN_POINT('',(2.225,4.,2.9));
#19654=CARTESIAN_POINT('Origin',(2.5,4.,3.8));
#19655=CARTESIAN_POINT('Origin',(2.5,-4.,2.9));
#19656=CARTESIAN_POINT('',(2.225,-4.,3.));
#19657=CARTESIAN_POINT('Origin',(2.5,-4.,3.));
#19658=CARTESIAN_POINT('',(2.225,-4.,3.8));
#19659=CARTESIAN_POINT('',(2.225,-4.,2.9));
#19660=CARTESIAN_POINT('Origin',(2.5,-4.,3.8));
#19661=CARTESIAN_POINT('Origin',(28.,6.,3.));
#19662=CARTESIAN_POINT('',(28.,6.,3.));
#19663=CARTESIAN_POINT('',(-6.,6.,3.));
#19664=CARTESIAN_POINT('',(28.,6.,3.));
#19665=CARTESIAN_POINT('',(-6.,6.,3.8));
#19666=CARTESIAN_POINT('',(-6.,6.,3.));
#19667=CARTESIAN_POINT('',(28.,6.,3.8));
#19668=CARTESIAN_POINT('',(28.,6.,3.8));
#19669=CARTESIAN_POINT('',(28.,6.,3.));
#19670=CARTESIAN_POINT('Origin',(28.,-6.,3.));
#19671=CARTESIAN_POINT('',(28.,-6.,3.));
#19672=CARTESIAN_POINT('',(28.,-6.,3.));
#19673=CARTESIAN_POINT('',(28.,-6.,3.8));
#19674=CARTESIAN_POINT('',(28.,-6.,3.8));
#19675=CARTESIAN_POINT('',(28.,-6.,3.));
#19676=CARTESIAN_POINT('Origin',(-6.,-6.,3.));
#19677=CARTESIAN_POINT('',(-6.,-6.,3.));
#19678=CARTESIAN_POINT('',(-6.,-6.,3.));
#19679=CARTESIAN_POINT('',(-6.,-6.,3.8));
#19680=CARTESIAN_POINT('',(-6.,-6.,3.8));
#19681=CARTESIAN_POINT('',(-6.,-6.,3.));
#19682=CARTESIAN_POINT('Origin',(-6.,6.,3.));
#19683=CARTESIAN_POINT('',(-6.,6.,3.));
#19684=CARTESIAN_POINT('',(-6.,6.,3.8));
#19685=CARTESIAN_POINT('Origin',(11.,0.,3.8));
#19686=CARTESIAN_POINT('Origin',(11.,0.,3.));
#19687=CARTESIAN_POINT('',(0.,0.,0.));
#19688=CARTESIAN_POINT('Origin',(-4.2,-1.8,4.8));
#19689=CARTESIAN_POINT('',(-4.7,-1.8,4.8));
#19690=CARTESIAN_POINT('Origin',(-4.2,-1.8,4.8));
#19691=CARTESIAN_POINT('',(-4.7,-1.8,7.));
#19692=CARTESIAN_POINT('',(-4.7,-1.8,4.8));
#19693=CARTESIAN_POINT('Origin',(-4.2,-1.8,7.));
#19694=CARTESIAN_POINT('Origin',(-4.2,-1.8,4.8));
#19695=CARTESIAN_POINT('',(-4.475,-1.8,4.8));
#19696=CARTESIAN_POINT('Origin',(-4.2,-1.8,4.8));
#19697=CARTESIAN_POINT('Origin',(-4.2,1.8,4.8));
#19698=CARTESIAN_POINT('',(-4.7,1.8,4.8));
#19699=CARTESIAN_POINT('Origin',(-4.2,1.8,4.8));
#19700=CARTESIAN_POINT('',(-4.7,1.8,7.));
#19701=CARTESIAN_POINT('',(-4.7,1.8,4.8));
#19702=CARTESIAN_POINT('Origin',(-4.2,1.8,7.));
#19703=CARTESIAN_POINT('Origin',(-4.2,1.8,4.8));
#19704=CARTESIAN_POINT('',(-4.475,1.8,4.8));
#19705=CARTESIAN_POINT('Origin',(-4.2,1.8,4.8));
#19706=CARTESIAN_POINT('Origin',(-4.2,-1.8,3.7));
#19707=CARTESIAN_POINT('',(-4.475,-1.8,3.8));
#19708=CARTESIAN_POINT('Origin',(-4.2,-1.8,3.8));
#19709=CARTESIAN_POINT('',(-4.475,-1.8,3.7));
#19710=CARTESIAN_POINT('Origin',(-4.2,1.8,3.7));
#19711=CARTESIAN_POINT('',(-4.475,1.8,3.8));
#19712=CARTESIAN_POINT('Origin',(-4.2,1.8,3.8));
#19713=CARTESIAN_POINT('',(-4.475,1.8,3.7));
#19714=CARTESIAN_POINT('Origin',(-3.2,2.5,3.8));
#19715=CARTESIAN_POINT('',(-3.2,2.5,3.8));
#19716=CARTESIAN_POINT('',(-5.2,2.5,3.8));
#19717=CARTESIAN_POINT('',(-3.2,2.5,3.8));
#19718=CARTESIAN_POINT('',(-5.2,2.5,7.));
#19719=CARTESIAN_POINT('',(-5.2,2.5,3.8));
#19720=CARTESIAN_POINT('',(-3.2,2.5,7.));
#19721=CARTESIAN_POINT('',(-3.2,2.5,7.));
#19722=CARTESIAN_POINT('',(-3.2,2.5,3.8));
#19723=CARTESIAN_POINT('Origin',(-3.2,-2.5,3.8));
#19724=CARTESIAN_POINT('',(-3.2,-2.5,3.8));
#19725=CARTESIAN_POINT('',(-3.2,-2.5,3.8));
#19726=CARTESIAN_POINT('',(-3.2,-2.5,7.));
#19727=CARTESIAN_POINT('',(-3.2,-2.5,7.));
#19728=CARTESIAN_POINT('',(-3.2,-2.5,3.8));
#19729=CARTESIAN_POINT('Origin',(-5.2,-2.5,3.8));
#19730=CARTESIAN_POINT('',(-5.2,-2.5,3.8));
#19731=CARTESIAN_POINT('',(-5.2,-2.5,3.8));
#19732=CARTESIAN_POINT('',(-5.2,-2.5,7.));
#19733=CARTESIAN_POINT('',(-5.2,-2.5,7.));
#19734=CARTESIAN_POINT('',(-5.2,-2.5,3.8));
#19735=CARTESIAN_POINT('Origin',(-5.2,2.5,3.8));
#19736=CARTESIAN_POINT('',(-5.2,2.5,3.8));
#19737=CARTESIAN_POINT('',(-5.2,2.5,7.));
#19738=CARTESIAN_POINT('Origin',(-4.2,0.,7.));
#19739=CARTESIAN_POINT('Origin',(-4.2,0.,3.8));
#19740=CARTESIAN_POINT('',(0.,0.,0.));
#19741=CARTESIAN_POINT('Origin',(-3.,2.5,6.2));
#19742=CARTESIAN_POINT('',(-3.,2.5,6.2));
#19743=CARTESIAN_POINT('',(-3.2,2.5,6.2));
#19744=CARTESIAN_POINT('',(-3.,2.5,6.2));
#19745=CARTESIAN_POINT('',(-3.2,2.5,7.));
#19746=CARTESIAN_POINT('',(-3.2,2.5,6.2));
#19747=CARTESIAN_POINT('',(-3.,2.5,7.));
#19748=CARTESIAN_POINT('',(-3.,2.5,7.));
#19749=CARTESIAN_POINT('',(-3.,2.5,6.2));
#19750=CARTESIAN_POINT('Origin',(-3.,-2.5,6.2));
#19751=CARTESIAN_POINT('',(-3.,-2.5,6.2));
#19752=CARTESIAN_POINT('',(-3.,-2.5,6.2));
#19753=CARTESIAN_POINT('',(-3.,-2.5,7.));
#19754=CARTESIAN_POINT('',(-3.,-2.5,7.));
#19755=CARTESIAN_POINT('',(-3.,-2.5,6.2));
#19756=CARTESIAN_POINT('Origin',(-3.2,-2.5,6.2));
#19757=CARTESIAN_POINT('',(-3.2,-2.5,6.2));
#19758=CARTESIAN_POINT('',(-3.2,-2.5,6.2));
#19759=CARTESIAN_POINT('',(-3.2,-2.5,7.));
#19760=CARTESIAN_POINT('',(-3.2,-2.5,7.));
#19761=CARTESIAN_POINT('',(-3.2,-2.5,6.2));
#19762=CARTESIAN_POINT('Origin',(-3.2,2.5,6.2));
#19763=CARTESIAN_POINT('',(-3.2,2.5,6.2));
#19764=CARTESIAN_POINT('',(-3.2,2.5,7.));
#19765=CARTESIAN_POINT('Origin',(-3.1,0.,7.));
#19766=CARTESIAN_POINT('Origin',(-3.1,0.,6.2));
#19767=CARTESIAN_POINT('',(0.,0.,0.));
#19768=CARTESIAN_POINT('Origin',(26.2,-1.8,4.8));
#19769=CARTESIAN_POINT('',(25.7,-1.8,4.8));
#19770=CARTESIAN_POINT('Origin',(26.2,-1.8,4.8));
#19771=CARTESIAN_POINT('',(25.7,-1.8,7.));
#19772=CARTESIAN_POINT('',(25.7,-1.8,4.8));
#19773=CARTESIAN_POINT('Origin',(26.2,-1.8,7.));
#19774=CARTESIAN_POINT('Origin',(26.2,-1.8,4.8));
#19775=CARTESIAN_POINT('',(25.925,-1.8,4.8));
#19776=CARTESIAN_POINT('Origin',(26.2,-1.8,4.8));
#19777=CARTESIAN_POINT('Origin',(26.2,1.8,4.8));
#19778=CARTESIAN_POINT('',(25.7,1.8,4.8));
#19779=CARTESIAN_POINT('Origin',(26.2,1.8,4.8));
#19780=CARTESIAN_POINT('',(25.7,1.8,7.));
#19781=CARTESIAN_POINT('',(25.7,1.8,4.8));
#19782=CARTESIAN_POINT('Origin',(26.2,1.8,7.));
#19783=CARTESIAN_POINT('Origin',(26.2,1.8,4.8));
#19784=CARTESIAN_POINT('',(25.925,1.8,4.8));
#19785=CARTESIAN_POINT('Origin',(26.2,1.8,4.8));
#19786=CARTESIAN_POINT('Origin',(26.2,-1.8,3.7));
#19787=CARTESIAN_POINT('',(25.925,-1.8,3.8));
#19788=CARTESIAN_POINT('Origin',(26.2,-1.8,3.8));
#19789=CARTESIAN_POINT('',(25.925,-1.8,3.7));
#19790=CARTESIAN_POINT('Origin',(26.2,1.8,3.7));
#19791=CARTESIAN_POINT('',(25.925,1.8,3.8));
#19792=CARTESIAN_POINT('Origin',(26.2,1.8,3.8));
#19793=CARTESIAN_POINT('',(25.925,1.8,3.7));
#19794=CARTESIAN_POINT('Origin',(27.2,2.5,3.8));
#19795=CARTESIAN_POINT('',(27.2,2.5,3.8));
#19796=CARTESIAN_POINT('',(25.2,2.5,3.8));
#19797=CARTESIAN_POINT('',(27.2,2.5,3.8));
#19798=CARTESIAN_POINT('',(25.2,2.5,7.));
#19799=CARTESIAN_POINT('',(25.2,2.5,3.8));
#19800=CARTESIAN_POINT('',(27.2,2.5,7.));
#19801=CARTESIAN_POINT('',(27.2,2.5,7.));
#19802=CARTESIAN_POINT('',(27.2,2.5,3.8));
#19803=CARTESIAN_POINT('Origin',(27.2,-2.5,3.8));
#19804=CARTESIAN_POINT('',(27.2,-2.5,3.8));
#19805=CARTESIAN_POINT('',(27.2,-2.5,3.8));
#19806=CARTESIAN_POINT('',(27.2,-2.5,7.));
#19807=CARTESIAN_POINT('',(27.2,-2.5,7.));
#19808=CARTESIAN_POINT('',(27.2,-2.5,3.8));
#19809=CARTESIAN_POINT('Origin',(25.2,-2.5,3.8));
#19810=CARTESIAN_POINT('',(25.2,-2.5,3.8));
#19811=CARTESIAN_POINT('',(25.2,-2.5,3.8));
#19812=CARTESIAN_POINT('',(25.2,-2.5,7.));
#19813=CARTESIAN_POINT('',(25.2,-2.5,7.));
#19814=CARTESIAN_POINT('',(25.2,-2.5,3.8));
#19815=CARTESIAN_POINT('Origin',(25.2,2.5,3.8));
#19816=CARTESIAN_POINT('',(25.2,2.5,3.8));
#19817=CARTESIAN_POINT('',(25.2,2.5,7.));
#19818=CARTESIAN_POINT('Origin',(26.2,0.,7.));
#19819=CARTESIAN_POINT('Origin',(26.2,0.,3.8));
#19820=CARTESIAN_POINT('',(0.,0.,0.));
#19821=CARTESIAN_POINT('Origin',(25.2,2.5,6.2));
#19822=CARTESIAN_POINT('',(25.2,2.5,6.2));
#19823=CARTESIAN_POINT('',(25.,2.5,6.2));
#19824=CARTESIAN_POINT('',(25.2,2.5,6.2));
#19825=CARTESIAN_POINT('',(25.,2.5,7.));
#19826=CARTESIAN_POINT('',(25.,2.5,6.2));
#19827=CARTESIAN_POINT('',(25.2,2.5,7.));
#19828=CARTESIAN_POINT('',(25.2,2.5,7.));
#19829=CARTESIAN_POINT('',(25.2,2.5,6.2));
#19830=CARTESIAN_POINT('Origin',(25.2,-2.5,6.2));
#19831=CARTESIAN_POINT('',(25.2,-2.5,6.2));
#19832=CARTESIAN_POINT('',(25.2,-2.5,6.2));
#19833=CARTESIAN_POINT('',(25.2,-2.5,7.));
#19834=CARTESIAN_POINT('',(25.2,-2.5,7.));
#19835=CARTESIAN_POINT('',(25.2,-2.5,6.2));
#19836=CARTESIAN_POINT('Origin',(25.,-2.5,6.2));
#19837=CARTESIAN_POINT('',(25.,-2.5,6.2));
#19838=CARTESIAN_POINT('',(25.,-2.5,6.2));
#19839=CARTESIAN_POINT('',(25.,-2.5,7.));
#19840=CARTESIAN_POINT('',(25.,-2.5,7.));
#19841=CARTESIAN_POINT('',(25.,-2.5,6.2));
#19842=CARTESIAN_POINT('Origin',(25.,2.5,6.2));
#19843=CARTESIAN_POINT('',(25.,2.5,6.2));
#19844=CARTESIAN_POINT('',(25.,2.5,7.));
#19845=CARTESIAN_POINT('Origin',(25.1,0.,7.));
#19846=CARTESIAN_POINT('Origin',(25.1,0.,6.2));
#19847=CARTESIAN_POINT('',(0.,0.,0.));
#19848=CARTESIAN_POINT('Origin',(8.,-4.2,3.7));
#19849=CARTESIAN_POINT('',(7.775,-4.2,3.8));
#19850=CARTESIAN_POINT('Origin',(8.,-4.2,3.8));
#19851=CARTESIAN_POINT('',(7.775,-4.2,4.6));
#19852=CARTESIAN_POINT('',(7.775,-4.2,3.7));
#19853=CARTESIAN_POINT('Origin',(8.,-4.2,4.6));
#19854=CARTESIAN_POINT('Origin',(14.,-4.2,3.7));
#19855=CARTESIAN_POINT('',(13.775,-4.2,3.8));
#19856=CARTESIAN_POINT('Origin',(14.,-4.2,3.8));
#19857=CARTESIAN_POINT('',(13.775,-4.2,4.6));
#19858=CARTESIAN_POINT('',(13.775,-4.2,3.7));
#19859=CARTESIAN_POINT('Origin',(14.,-4.2,4.6));
#19860=CARTESIAN_POINT('Origin',(9.51507575950825,-5.1,8.76507575950825));
#19861=CARTESIAN_POINT('',(9.35007575950825,-5.,8.76507575950825));
#19862=CARTESIAN_POINT('Origin',(9.51507575950825,-5.,8.76507575950825));
#19863=CARTESIAN_POINT('',(9.35007575950825,-3.4,8.76507575950825));
#19864=CARTESIAN_POINT('',(9.35007575950825,-5.1,8.76507575950825));
#19865=CARTESIAN_POINT('Origin',(9.51507575950825,-3.4,8.76507575950825));
#19866=CARTESIAN_POINT('Origin',(9.51507575950825,-5.1,11.7349242404918));
#19867=CARTESIAN_POINT('',(9.35007575950825,-5.,11.7349242404918));
#19868=CARTESIAN_POINT('Origin',(9.51507575950825,-5.,11.7349242404918));
#19869=CARTESIAN_POINT('',(9.35007575950825,-3.4,11.7349242404918));
#19870=CARTESIAN_POINT('',(9.35007575950825,-5.1,11.7349242404918));
#19871=CARTESIAN_POINT('Origin',(9.51507575950825,-3.4,11.7349242404918));
#19872=CARTESIAN_POINT('Origin',(12.4849242404918,-5.1,11.7349242404918));
#19873=CARTESIAN_POINT('',(12.3199242404918,-5.,11.7349242404918));
#19874=CARTESIAN_POINT('Origin',(12.4849242404918,-5.,11.7349242404918));
#19875=CARTESIAN_POINT('',(12.3199242404918,-3.4,11.7349242404918));
#19876=CARTESIAN_POINT('',(12.3199242404918,-5.1,11.7349242404918));
#19877=CARTESIAN_POINT('Origin',(12.4849242404918,-3.4,11.7349242404918));
#19878=CARTESIAN_POINT('Origin',(12.4849242404917,-5.1,8.76507575950825));
#19879=CARTESIAN_POINT('',(12.3199242404917,-5.,8.76507575950825));
#19880=CARTESIAN_POINT('Origin',(12.4849242404917,-5.,8.76507575950825));
#19881=CARTESIAN_POINT('',(12.3199242404917,-3.4,8.76507575950825));
#19882=CARTESIAN_POINT('',(12.3199242404917,-5.1,8.76507575950825));
#19883=CARTESIAN_POINT('Origin',(12.4849242404917,-3.4,8.76507575950825));
#19884=CARTESIAN_POINT('Origin',(11.,-5.1,10.25));
#19885=CARTESIAN_POINT('',(9.4,-5.,10.25));
#19886=CARTESIAN_POINT('Origin',(11.,-5.,10.25));
#19887=CARTESIAN_POINT('',(9.4,-3.4,10.25));
#19888=CARTESIAN_POINT('',(9.4,-5.1,10.25));
#19889=CARTESIAN_POINT('Origin',(11.,-3.4,10.25));
#19890=CARTESIAN_POINT('Origin',(7.4,-5.,4.6));
#19891=CARTESIAN_POINT('',(13.4,-5.,4.6));
#19892=CARTESIAN_POINT('',(13.4,-3.4,4.6));
#19893=CARTESIAN_POINT('',(13.4,-5.,4.6));
#19894=CARTESIAN_POINT('',(14.6,-5.,4.6));
#19895=CARTESIAN_POINT('',(14.6,-5.,4.6));
#19896=CARTESIAN_POINT('',(14.6,-3.4,4.6));
#19897=CARTESIAN_POINT('',(14.6,-5.,4.6));
#19898=CARTESIAN_POINT('',(14.6,-3.4,4.6));
#19899=CARTESIAN_POINT('Origin',(7.4,-5.,4.6));
#19900=CARTESIAN_POINT('',(8.6,-3.4,4.6));
#19901=CARTESIAN_POINT('',(8.6,-5.,4.6));
#19902=CARTESIAN_POINT('',(8.6,-4.2,4.6));
#19903=CARTESIAN_POINT('',(7.4,-3.4,4.6));
#19904=CARTESIAN_POINT('',(14.6,-3.4,4.6));
#19905=CARTESIAN_POINT('',(7.4,-5.,4.6));
#19906=CARTESIAN_POINT('',(7.4,-5.,4.6));
#19907=CARTESIAN_POINT('',(14.6,-5.,4.6));
#19908=CARTESIAN_POINT('Origin',(7.4,-5.,3.8));
#19909=CARTESIAN_POINT('',(7.4,-5.,3.8));
#19910=CARTESIAN_POINT('',(7.4,-5.,4.6));
#19911=CARTESIAN_POINT('',(7.4,-3.4,3.8));
#19912=CARTESIAN_POINT('',(7.4,-3.4,4.6));
#19913=CARTESIAN_POINT('',(7.4,-5.,3.8));
#19914=CARTESIAN_POINT('Origin',(14.6,-5.,4.6));
#19915=CARTESIAN_POINT('',(14.6,-5.,3.8));
#19916=CARTESIAN_POINT('',(14.6,-5.,3.8));
#19917=CARTESIAN_POINT('',(14.6,-3.4,3.8));
#19918=CARTESIAN_POINT('',(14.6,-5.,3.8));
#19919=CARTESIAN_POINT('',(14.6,-3.4,3.8));
#19920=CARTESIAN_POINT('Origin',(8.6,-5.,3.8));
#19921=CARTESIAN_POINT('',(13.4,-5.,12.7));
#19922=CARTESIAN_POINT('',(13.4,-5.,3.8));
#19923=CARTESIAN_POINT('',(8.6,-5.,12.7));
#19924=CARTESIAN_POINT('',(8.6,-5.,12.7));
#19925=CARTESIAN_POINT('',(8.6,-5.,3.8));
#19926=CARTESIAN_POINT('',(7.4,-5.,3.8));
#19927=CARTESIAN_POINT('Origin',(13.4,-5.,3.8));
#19928=CARTESIAN_POINT('',(13.4,-3.4,12.7));
#19929=CARTESIAN_POINT('',(13.4,-3.4,3.8));
#19930=CARTESIAN_POINT('',(13.4,-5.,12.7));
#19931=CARTESIAN_POINT('Origin',(13.4,-3.4,3.8));
#19932=CARTESIAN_POINT('',(8.6,-3.4,12.7));
#19933=CARTESIAN_POINT('',(8.6,-3.4,3.8));
#19934=CARTESIAN_POINT('',(13.4,-3.4,12.7));
#19935=CARTESIAN_POINT('',(7.4,-3.4,3.8));
#19936=CARTESIAN_POINT('Origin',(8.6,-3.4,3.8));
#19937=CARTESIAN_POINT('',(8.6,-3.4,12.7));
#19938=CARTESIAN_POINT('Origin',(11.,-4.2,12.7));
#19939=CARTESIAN_POINT('Origin',(11.,-4.2,3.8));
#19940=CARTESIAN_POINT('',(0.,0.,0.));
#19941=CARTESIAN_POINT('Origin',(9.51507575950825,-5.3,8.76507575950825));
#19942=CARTESIAN_POINT('',(9.29007575950825,-5.2,8.76507575950825));
#19943=CARTESIAN_POINT('Origin',(9.51507575950825,-5.2,8.76507575950825));
#19944=CARTESIAN_POINT('',(9.29007575950825,-5.,8.76507575950825));
#19945=CARTESIAN_POINT('',(9.29007575950825,-5.3,8.76507575950825));
#19946=CARTESIAN_POINT('Origin',(9.51507575950825,-5.,8.76507575950825));
#19947=CARTESIAN_POINT('Origin',(9.51507575950825,-5.3,11.7349242404918));
#19948=CARTESIAN_POINT('',(9.29007575950825,-5.2,11.7349242404918));
#19949=CARTESIAN_POINT('Origin',(9.51507575950825,-5.2,11.7349242404918));
#19950=CARTESIAN_POINT('',(9.29007575950825,-5.,11.7349242404918));
#19951=CARTESIAN_POINT('',(9.29007575950825,-5.3,11.7349242404918));
#19952=CARTESIAN_POINT('Origin',(9.51507575950825,-5.,11.7349242404918));
#19953=CARTESIAN_POINT('Origin',(12.4849242404918,-5.3,11.7349242404918));
#19954=CARTESIAN_POINT('',(12.2599242404918,-5.2,11.7349242404918));
#19955=CARTESIAN_POINT('Origin',(12.4849242404918,-5.2,11.7349242404918));
#19956=CARTESIAN_POINT('',(12.2599242404918,-5.,11.7349242404918));
#19957=CARTESIAN_POINT('',(12.2599242404918,-5.3,11.7349242404918));
#19958=CARTESIAN_POINT('Origin',(12.4849242404918,-5.,11.7349242404918));
#19959=CARTESIAN_POINT('Origin',(12.4849242404917,-5.3,8.76507575950825));
#19960=CARTESIAN_POINT('',(12.2599242404917,-5.2,8.76507575950825));
#19961=CARTESIAN_POINT('Origin',(12.4849242404917,-5.2,8.76507575950825));
#19962=CARTESIAN_POINT('',(12.2599242404917,-5.,8.76507575950825));
#19963=CARTESIAN_POINT('',(12.2599242404917,-5.3,8.76507575950825));
#19964=CARTESIAN_POINT('Origin',(12.4849242404917,-5.,8.76507575950825));
#19965=CARTESIAN_POINT('Origin',(11.,-5.,10.25));
#19966=CARTESIAN_POINT('',(9.41,-4.7,10.25));
#19967=CARTESIAN_POINT('Origin',(11.,-4.7,10.25));
#19968=CARTESIAN_POINT('',(9.41,-5.,10.25));
#19969=CARTESIAN_POINT('',(9.41,-5.,10.25));
#19970=CARTESIAN_POINT('Origin',(11.,-5.,10.25));
#19971=CARTESIAN_POINT('Origin',(11.,-4.7,10.25));
#19972=CARTESIAN_POINT('',(9.8,-4.7,10.25));
#19973=CARTESIAN_POINT('Origin',(11.,-4.7,10.25));
#19974=CARTESIAN_POINT('Origin',(11.,-5.2,10.25));
#19975=CARTESIAN_POINT('',(9.8,-5.2,10.25));
#19976=CARTESIAN_POINT('',(9.8,-5.2,10.25));
#19977=CARTESIAN_POINT('Origin',(11.,-5.2,10.25));
#19978=CARTESIAN_POINT('Origin',(11.,-5.2,10.25));
#19979=CARTESIAN_POINT('',(8.6,-5.,10.25));
#19980=CARTESIAN_POINT('Origin',(11.,-5.,10.25));
#19981=CARTESIAN_POINT('',(8.6,-5.2,10.25));
#19982=CARTESIAN_POINT('',(8.6,-5.2,10.25));
#19983=CARTESIAN_POINT('Origin',(11.,-5.2,10.25));
#19984=CARTESIAN_POINT('Origin',(11.,-5.,10.25));
#19985=CARTESIAN_POINT('Origin',(11.,-5.2,10.25));
#19986=CARTESIAN_POINT('',(0.,0.,0.));
#19987=CARTESIAN_POINT('Origin',(9.51507575950825,-3.5,8.76507575950825));
#19988=CARTESIAN_POINT('',(9.29007575950825,-3.4,8.76507575950825));
#19989=CARTESIAN_POINT('Origin',(9.51507575950825,-3.4,8.76507575950825));
#19990=CARTESIAN_POINT('',(9.29007575950825,-3.2,8.76507575950825));
#19991=CARTESIAN_POINT('',(9.29007575950825,-3.5,8.76507575950825));
#19992=CARTESIAN_POINT('Origin',(9.51507575950825,-3.2,8.76507575950825));
#19993=CARTESIAN_POINT('Origin',(9.51507575950825,-3.5,11.7349242404918));
#19994=CARTESIAN_POINT('',(9.29007575950825,-3.4,11.7349242404918));
#19995=CARTESIAN_POINT('Origin',(9.51507575950825,-3.4,11.7349242404918));
#19996=CARTESIAN_POINT('',(9.29007575950825,-3.2,11.7349242404918));
#19997=CARTESIAN_POINT('',(9.29007575950825,-3.5,11.7349242404918));
#19998=CARTESIAN_POINT('Origin',(9.51507575950825,-3.2,11.7349242404918));
#19999=CARTESIAN_POINT('Origin',(12.4849242404918,-3.5,11.7349242404918));
#20000=CARTESIAN_POINT('',(12.2599242404918,-3.4,11.7349242404918));
#20001=CARTESIAN_POINT('Origin',(12.4849242404918,-3.4,11.7349242404918));
#20002=CARTESIAN_POINT('',(12.2599242404918,-3.2,11.7349242404918));
#20003=CARTESIAN_POINT('',(12.2599242404918,-3.5,11.7349242404918));
#20004=CARTESIAN_POINT('Origin',(12.4849242404918,-3.2,11.7349242404918));
#20005=CARTESIAN_POINT('Origin',(12.4849242404917,-3.5,8.76507575950825));
#20006=CARTESIAN_POINT('',(12.2599242404917,-3.4,8.76507575950825));
#20007=CARTESIAN_POINT('Origin',(12.4849242404917,-3.4,8.76507575950825));
#20008=CARTESIAN_POINT('',(12.2599242404917,-3.2,8.76507575950825));
#20009=CARTESIAN_POINT('',(12.2599242404917,-3.5,8.76507575950825));
#20010=CARTESIAN_POINT('Origin',(12.4849242404917,-3.2,8.76507575950825));
#20011=CARTESIAN_POINT('Origin',(11.,-3.7,10.25));
#20012=CARTESIAN_POINT('',(9.41,-3.4,10.25));
#20013=CARTESIAN_POINT('Origin',(11.,-3.4,10.25));
#20014=CARTESIAN_POINT('',(9.41,-3.7,10.25));
#20015=CARTESIAN_POINT('',(9.41,-3.7,10.25));
#20016=CARTESIAN_POINT('Origin',(11.,-3.7,10.25));
#20017=CARTESIAN_POINT('Origin',(11.,-3.7,10.25));
#20018=CARTESIAN_POINT('',(9.8,-3.7,10.25));
#20019=CARTESIAN_POINT('Origin',(11.,-3.7,10.25));
#20020=CARTESIAN_POINT('Origin',(11.,-3.4,10.25));
#20021=CARTESIAN_POINT('',(9.8,-3.2,10.25));
#20022=CARTESIAN_POINT('Origin',(11.,-3.2,10.25));
#20023=CARTESIAN_POINT('',(9.8,-3.4,10.25));
#20024=CARTESIAN_POINT('Origin',(11.,-3.4,10.25));
#20025=CARTESIAN_POINT('',(8.6,-3.2,10.25));
#20026=CARTESIAN_POINT('Origin',(11.,-3.2,10.25));
#20027=CARTESIAN_POINT('',(8.6,-3.4,10.25));
#20028=CARTESIAN_POINT('',(8.6,-3.4,10.25));
#20029=CARTESIAN_POINT('Origin',(11.,-3.4,10.25));
#20030=CARTESIAN_POINT('Origin',(11.,-3.2,10.25));
#20031=CARTESIAN_POINT('Origin',(11.,-3.4,10.25));
#20032=CARTESIAN_POINT('',(0.,0.,0.));
#20033=CARTESIAN_POINT('Origin',(8.,4.2,3.7));
#20034=CARTESIAN_POINT('',(7.775,4.2,3.8));
#20035=CARTESIAN_POINT('Origin',(8.,4.2,3.8));
#20036=CARTESIAN_POINT('',(7.775,4.2,4.6));
#20037=CARTESIAN_POINT('',(7.775,4.2,3.7));
#20038=CARTESIAN_POINT('Origin',(8.,4.2,4.6));
#20039=CARTESIAN_POINT('Origin',(14.,4.2,3.7));
#20040=CARTESIAN_POINT('',(13.775,4.2,3.8));
#20041=CARTESIAN_POINT('Origin',(14.,4.2,3.8));
#20042=CARTESIAN_POINT('',(13.775,4.2,4.6));
#20043=CARTESIAN_POINT('',(13.775,4.2,3.7));
#20044=CARTESIAN_POINT('Origin',(14.,4.2,4.6));
#20045=CARTESIAN_POINT('Origin',(9.51507575950825,3.3,8.76507575950825));
#20046=CARTESIAN_POINT('',(9.35007575950825,3.4,8.76507575950825));
#20047=CARTESIAN_POINT('Origin',(9.51507575950825,3.4,8.76507575950825));
#20048=CARTESIAN_POINT('',(9.35007575950825,5.,8.76507575950825));
#20049=CARTESIAN_POINT('',(9.35007575950825,3.3,8.76507575950825));
#20050=CARTESIAN_POINT('Origin',(9.51507575950825,5.,8.76507575950825));
#20051=CARTESIAN_POINT('Origin',(9.51507575950825,3.3,11.7349242404918));
#20052=CARTESIAN_POINT('',(9.35007575950825,3.4,11.7349242404918));
#20053=CARTESIAN_POINT('Origin',(9.51507575950825,3.4,11.7349242404918));
#20054=CARTESIAN_POINT('',(9.35007575950825,5.,11.7349242404918));
#20055=CARTESIAN_POINT('',(9.35007575950825,3.3,11.7349242404918));
#20056=CARTESIAN_POINT('Origin',(9.51507575950825,5.,11.7349242404918));
#20057=CARTESIAN_POINT('Origin',(12.4849242404918,3.3,11.7349242404918));
#20058=CARTESIAN_POINT('',(12.3199242404918,3.4,11.7349242404918));
#20059=CARTESIAN_POINT('Origin',(12.4849242404918,3.4,11.7349242404918));
#20060=CARTESIAN_POINT('',(12.3199242404918,5.,11.7349242404918));
#20061=CARTESIAN_POINT('',(12.3199242404918,3.3,11.7349242404918));
#20062=CARTESIAN_POINT('Origin',(12.4849242404918,5.,11.7349242404918));
#20063=CARTESIAN_POINT('Origin',(12.4849242404917,3.3,8.76507575950825));
#20064=CARTESIAN_POINT('',(12.3199242404917,3.4,8.76507575950825));
#20065=CARTESIAN_POINT('Origin',(12.4849242404917,3.4,8.76507575950825));
#20066=CARTESIAN_POINT('',(12.3199242404917,5.,8.76507575950825));
#20067=CARTESIAN_POINT('',(12.3199242404917,3.3,8.76507575950825));
#20068=CARTESIAN_POINT('Origin',(12.4849242404917,5.,8.76507575950825));
#20069=CARTESIAN_POINT('Origin',(11.,3.3,10.25));
#20070=CARTESIAN_POINT('',(9.4,3.4,10.25));
#20071=CARTESIAN_POINT('Origin',(11.,3.4,10.25));
#20072=CARTESIAN_POINT('',(9.4,5.,10.25));
#20073=CARTESIAN_POINT('',(9.4,3.3,10.25));
#20074=CARTESIAN_POINT('Origin',(11.,5.,10.25));
#20075=CARTESIAN_POINT('Origin',(7.4,3.4,4.6));
#20076=CARTESIAN_POINT('',(13.4,3.4,4.6));
#20077=CARTESIAN_POINT('',(13.4,5.,4.6));
#20078=CARTESIAN_POINT('',(13.4,3.4,4.6));
#20079=CARTESIAN_POINT('',(14.6,3.4,4.6));
#20080=CARTESIAN_POINT('',(14.6,3.4,4.6));
#20081=CARTESIAN_POINT('',(14.6,5.,4.6));
#20082=CARTESIAN_POINT('',(14.6,3.4,4.6));
#20083=CARTESIAN_POINT('',(14.6,5.,4.6));
#20084=CARTESIAN_POINT('Origin',(7.4,3.4,4.6));
#20085=CARTESIAN_POINT('',(8.6,5.,4.6));
#20086=CARTESIAN_POINT('',(8.6,3.4,4.6));
#20087=CARTESIAN_POINT('',(8.6,4.2,4.6));
#20088=CARTESIAN_POINT('',(7.4,5.,4.6));
#20089=CARTESIAN_POINT('',(14.6,5.,4.6));
#20090=CARTESIAN_POINT('',(7.4,3.4,4.6));
#20091=CARTESIAN_POINT('',(7.4,3.4,4.6));
#20092=CARTESIAN_POINT('',(14.6,3.4,4.6));
#20093=CARTESIAN_POINT('Origin',(7.4,3.4,3.8));
#20094=CARTESIAN_POINT('',(7.4,3.4,3.8));
#20095=CARTESIAN_POINT('',(7.4,3.4,4.6));
#20096=CARTESIAN_POINT('',(7.4,5.,3.8));
#20097=CARTESIAN_POINT('',(7.4,5.,4.6));
#20098=CARTESIAN_POINT('',(7.4,3.4,3.8));
#20099=CARTESIAN_POINT('Origin',(14.6,3.4,4.6));
#20100=CARTESIAN_POINT('',(14.6,3.4,3.8));
#20101=CARTESIAN_POINT('',(14.6,3.4,3.8));
#20102=CARTESIAN_POINT('',(14.6,5.,3.8));
#20103=CARTESIAN_POINT('',(14.6,3.4,3.8));
#20104=CARTESIAN_POINT('',(14.6,5.,3.8));
#20105=CARTESIAN_POINT('Origin',(8.6,3.4,3.8));
#20106=CARTESIAN_POINT('',(13.4,3.4,12.7));
#20107=CARTESIAN_POINT('',(13.4,3.4,3.8));
#20108=CARTESIAN_POINT('',(8.6,3.4,12.7));
#20109=CARTESIAN_POINT('',(8.6,3.4,12.7));
#20110=CARTESIAN_POINT('',(8.6,3.4,3.8));
#20111=CARTESIAN_POINT('',(7.4,3.4,3.8));
#20112=CARTESIAN_POINT('Origin',(13.4,3.4,3.8));
#20113=CARTESIAN_POINT('',(13.4,5.,12.7));
#20114=CARTESIAN_POINT('',(13.4,5.,3.8));
#20115=CARTESIAN_POINT('',(13.4,3.4,12.7));
#20116=CARTESIAN_POINT('Origin',(13.4,5.,3.8));
#20117=CARTESIAN_POINT('',(8.6,5.,12.7));
#20118=CARTESIAN_POINT('',(8.6,5.,3.8));
#20119=CARTESIAN_POINT('',(13.4,5.,12.7));
#20120=CARTESIAN_POINT('',(7.4,5.,3.8));
#20121=CARTESIAN_POINT('Origin',(8.6,5.,3.8));
#20122=CARTESIAN_POINT('',(8.6,5.,12.7));
#20123=CARTESIAN_POINT('Origin',(11.,4.2,12.7));
#20124=CARTESIAN_POINT('Origin',(11.,4.2,3.8));
#20125=CARTESIAN_POINT('',(0.,0.,0.));
#20126=CARTESIAN_POINT('Origin',(9.51507575950825,3.1,8.76507575950825));
#20127=CARTESIAN_POINT('',(9.29007575950825,3.2,8.76507575950825));
#20128=CARTESIAN_POINT('Origin',(9.51507575950825,3.2,8.76507575950825));
#20129=CARTESIAN_POINT('',(9.29007575950825,3.4,8.76507575950825));
#20130=CARTESIAN_POINT('',(9.29007575950825,3.1,8.76507575950825));
#20131=CARTESIAN_POINT('Origin',(9.51507575950825,3.4,8.76507575950825));
#20132=CARTESIAN_POINT('Origin',(9.51507575950825,3.1,11.7349242404918));
#20133=CARTESIAN_POINT('',(9.29007575950825,3.2,11.7349242404918));
#20134=CARTESIAN_POINT('Origin',(9.51507575950825,3.2,11.7349242404918));
#20135=CARTESIAN_POINT('',(9.29007575950825,3.4,11.7349242404918));
#20136=CARTESIAN_POINT('',(9.29007575950825,3.1,11.7349242404918));
#20137=CARTESIAN_POINT('Origin',(9.51507575950825,3.4,11.7349242404918));
#20138=CARTESIAN_POINT('Origin',(12.4849242404918,3.1,11.7349242404918));
#20139=CARTESIAN_POINT('',(12.2599242404918,3.2,11.7349242404918));
#20140=CARTESIAN_POINT('Origin',(12.4849242404918,3.2,11.7349242404918));
#20141=CARTESIAN_POINT('',(12.2599242404918,3.4,11.7349242404918));
#20142=CARTESIAN_POINT('',(12.2599242404918,3.1,11.7349242404918));
#20143=CARTESIAN_POINT('Origin',(12.4849242404918,3.4,11.7349242404918));
#20144=CARTESIAN_POINT('Origin',(12.4849242404917,3.1,8.76507575950825));
#20145=CARTESIAN_POINT('',(12.2599242404917,3.2,8.76507575950825));
#20146=CARTESIAN_POINT('Origin',(12.4849242404917,3.2,8.76507575950825));
#20147=CARTESIAN_POINT('',(12.2599242404917,3.4,8.76507575950825));
#20148=CARTESIAN_POINT('',(12.2599242404917,3.1,8.76507575950825));
#20149=CARTESIAN_POINT('Origin',(12.4849242404917,3.4,8.76507575950825));
#20150=CARTESIAN_POINT('Origin',(11.,3.4,10.25));
#20151=CARTESIAN_POINT('',(9.41,3.7,10.25));
#20152=CARTESIAN_POINT('Origin',(11.,3.7,10.25));
#20153=CARTESIAN_POINT('',(9.41,3.4,10.25));
#20154=CARTESIAN_POINT('',(9.41,3.4,10.25));
#20155=CARTESIAN_POINT('Origin',(11.,3.4,10.25));
#20156=CARTESIAN_POINT('Origin',(11.,3.7,10.25));
#20157=CARTESIAN_POINT('',(9.8,3.7,10.25));
#20158=CARTESIAN_POINT('Origin',(11.,3.7,10.25));
#20159=CARTESIAN_POINT('Origin',(11.,3.2,10.25));
#20160=CARTESIAN_POINT('',(9.8,3.2,10.25));
#20161=CARTESIAN_POINT('',(9.8,3.2,10.25));
#20162=CARTESIAN_POINT('Origin',(11.,3.2,10.25));
#20163=CARTESIAN_POINT('Origin',(11.,3.2,10.25));
#20164=CARTESIAN_POINT('',(8.6,3.4,10.25));
#20165=CARTESIAN_POINT('Origin',(11.,3.4,10.25));
#20166=CARTESIAN_POINT('',(8.6,3.2,10.25));
#20167=CARTESIAN_POINT('',(8.6,3.2,10.25));
#20168=CARTESIAN_POINT('Origin',(11.,3.2,10.25));
#20169=CARTESIAN_POINT('Origin',(11.,3.4,10.25));
#20170=CARTESIAN_POINT('Origin',(11.,3.2,10.25));
#20171=CARTESIAN_POINT('',(0.,0.,0.));
#20172=CARTESIAN_POINT('Origin',(9.51507575950825,4.9,8.76507575950825));
#20173=CARTESIAN_POINT('',(9.29007575950825,5.,8.76507575950825));
#20174=CARTESIAN_POINT('Origin',(9.51507575950825,5.,8.76507575950825));
#20175=CARTESIAN_POINT('',(9.29007575950825,5.2,8.76507575950825));
#20176=CARTESIAN_POINT('',(9.29007575950825,4.9,8.76507575950825));
#20177=CARTESIAN_POINT('Origin',(9.51507575950825,5.2,8.76507575950825));
#20178=CARTESIAN_POINT('Origin',(9.51507575950825,4.9,11.7349242404918));
#20179=CARTESIAN_POINT('',(9.29007575950825,5.,11.7349242404918));
#20180=CARTESIAN_POINT('Origin',(9.51507575950825,5.,11.7349242404918));
#20181=CARTESIAN_POINT('',(9.29007575950825,5.2,11.7349242404918));
#20182=CARTESIAN_POINT('',(9.29007575950825,4.9,11.7349242404918));
#20183=CARTESIAN_POINT('Origin',(9.51507575950825,5.2,11.7349242404918));
#20184=CARTESIAN_POINT('Origin',(12.4849242404918,4.9,11.7349242404918));
#20185=CARTESIAN_POINT('',(12.2599242404918,5.,11.7349242404918));
#20186=CARTESIAN_POINT('Origin',(12.4849242404918,5.,11.7349242404918));
#20187=CARTESIAN_POINT('',(12.2599242404918,5.2,11.7349242404918));
#20188=CARTESIAN_POINT('',(12.2599242404918,4.9,11.7349242404918));
#20189=CARTESIAN_POINT('Origin',(12.4849242404918,5.2,11.7349242404918));
#20190=CARTESIAN_POINT('Origin',(12.4849242404917,4.9,8.76507575950825));
#20191=CARTESIAN_POINT('',(12.2599242404917,5.,8.76507575950825));
#20192=CARTESIAN_POINT('Origin',(12.4849242404917,5.,8.76507575950825));
#20193=CARTESIAN_POINT('',(12.2599242404917,5.2,8.76507575950825));
#20194=CARTESIAN_POINT('',(12.2599242404917,4.9,8.76507575950825));
#20195=CARTESIAN_POINT('Origin',(12.4849242404917,5.2,8.76507575950825));
#20196=CARTESIAN_POINT('Origin',(11.,4.7,10.25));
#20197=CARTESIAN_POINT('',(9.41,5.,10.25));
#20198=CARTESIAN_POINT('Origin',(11.,5.,10.25));
#20199=CARTESIAN_POINT('',(9.41,4.7,10.25));
#20200=CARTESIAN_POINT('',(9.41,4.7,10.25));
#20201=CARTESIAN_POINT('Origin',(11.,4.7,10.25));
#20202=CARTESIAN_POINT('Origin',(11.,4.7,10.25));
#20203=CARTESIAN_POINT('',(9.8,4.7,10.25));
#20204=CARTESIAN_POINT('Origin',(11.,4.7,10.25));
#20205=CARTESIAN_POINT('Origin',(11.,5.,10.25));
#20206=CARTESIAN_POINT('',(9.8,5.2,10.25));
#20207=CARTESIAN_POINT('Origin',(11.,5.2,10.25));
#20208=CARTESIAN_POINT('',(9.8,5.,10.25));
#20209=CARTESIAN_POINT('Origin',(11.,5.,10.25));
#20210=CARTESIAN_POINT('',(8.6,5.2,10.25));
#20211=CARTESIAN_POINT('Origin',(11.,5.2,10.25));
#20212=CARTESIAN_POINT('',(8.6,5.,10.25));
#20213=CARTESIAN_POINT('',(8.6,5.,10.25));
#20214=CARTESIAN_POINT('Origin',(11.,5.,10.25));
#20215=CARTESIAN_POINT('Origin',(11.,5.2,10.25));
#20216=CARTESIAN_POINT('Origin',(11.,5.,10.25));
#20217=CARTESIAN_POINT('',(0.,0.,0.));
#20218=CARTESIAN_POINT('Origin',(-0.1,0.82,-0.3));
#20219=CARTESIAN_POINT('',(0.,0.82,-0.3));
#20220=CARTESIAN_POINT('',(0.,1.,-0.3));
#20221=CARTESIAN_POINT('',(0.,0.41,-0.3));
#20222=CARTESIAN_POINT('',(20.,0.82,-0.3));
#20223=CARTESIAN_POINT('',(-0.1,0.82,-0.3));
#20224=CARTESIAN_POINT('',(20.,1.,-0.3));
#20225=CARTESIAN_POINT('',(20.,0.41,-0.3));
#20226=CARTESIAN_POINT('',(-0.05,1.,-0.3));
#20227=CARTESIAN_POINT('Origin',(-0.1,0.82,-0.55));
#20228=CARTESIAN_POINT('',(0.,0.82,-0.55));
#20229=CARTESIAN_POINT('',(0.,0.82,-0.275));
#20230=CARTESIAN_POINT('',(20.,0.82,-0.55));
#20231=CARTESIAN_POINT('',(-0.1,0.82,-0.55));
#20232=CARTESIAN_POINT('',(20.,0.82,-0.275));
#20233=CARTESIAN_POINT('Origin',(-0.1,0.67,-0.55));
#20234=CARTESIAN_POINT('',(0.,0.67,-0.55));
#20235=CARTESIAN_POINT('',(0.,0.335,-0.55));
#20236=CARTESIAN_POINT('',(20.,0.67,-0.55));
#20237=CARTESIAN_POINT('',(-0.1,0.67,-0.55));
#20238=CARTESIAN_POINT('',(20.,0.335,-0.55));
#20239=CARTESIAN_POINT('Origin',(-0.1,0.42,-0.3));
#20240=CARTESIAN_POINT('',(0.,0.42,-0.3));
#20241=CARTESIAN_POINT('',(0.,0.24,-0.12));
#20242=CARTESIAN_POINT('',(20.,0.42,-0.3));
#20243=CARTESIAN_POINT('',(-0.1,0.42,-0.3));
#20244=CARTESIAN_POINT('',(20.,0.24,-0.12));
#20245=CARTESIAN_POINT('Origin',(-0.1,0.42,0.3));
#20246=CARTESIAN_POINT('',(0.,0.42,0.3));
#20247=CARTESIAN_POINT('',(0.,0.42,0.15));
#20248=CARTESIAN_POINT('',(20.,0.42,0.3));
#20249=CARTESIAN_POINT('',(-0.1,0.42,0.3));
#20250=CARTESIAN_POINT('',(20.,0.42,0.15));
#20251=CARTESIAN_POINT('Origin',(-0.1,0.67,0.55));
#20252=CARTESIAN_POINT('',(0.,0.67,0.55));
#20253=CARTESIAN_POINT('',(6.93889390390723E-18,0.365,0.245));
#20254=CARTESIAN_POINT('',(20.,0.67,0.55));
#20255=CARTESIAN_POINT('',(-0.1,0.67,0.55));
#20256=CARTESIAN_POINT('',(20.,0.365,0.245));
#20257=CARTESIAN_POINT('Origin',(-0.1,0.82,0.55));
#20258=CARTESIAN_POINT('',(0.,0.82,0.55));
#20259=CARTESIAN_POINT('',(0.,0.41,0.55));
#20260=CARTESIAN_POINT('',(20.,0.82,0.55));
#20261=CARTESIAN_POINT('',(-0.1,0.82,0.55));
#20262=CARTESIAN_POINT('',(20.,0.41,0.55));
#20263=CARTESIAN_POINT('Origin',(-0.1,0.82,0.3));
#20264=CARTESIAN_POINT('',(0.,0.82,0.3));
#20265=CARTESIAN_POINT('',(0.,0.82,0.15));
#20266=CARTESIAN_POINT('',(20.,0.82,0.3));
#20267=CARTESIAN_POINT('',(-0.1,0.82,0.3));
#20268=CARTESIAN_POINT('',(20.,0.82,0.15));
#20269=CARTESIAN_POINT('Origin',(-0.1,1.05,0.3));
#20270=CARTESIAN_POINT('',(0.,1.,0.3));
#20271=CARTESIAN_POINT('',(0.,0.525,0.3));
#20272=CARTESIAN_POINT('',(20.,1.,0.3));
#20273=CARTESIAN_POINT('',(-0.05,1.,0.3));
#20274=CARTESIAN_POINT('',(20.,0.525,0.3));
#20275=CARTESIAN_POINT('Origin',(-0.1,-0.3,-0.82));
#20276=CARTESIAN_POINT('',(0.,-0.3,-0.82));
#20277=CARTESIAN_POINT('',(0.,-0.3,-1.));
#20278=CARTESIAN_POINT('',(0.,-0.3,-0.41));
#20279=CARTESIAN_POINT('',(20.,-0.3,-0.82));
#20280=CARTESIAN_POINT('',(-0.1,-0.3,-0.82));
#20281=CARTESIAN_POINT('',(20.,-0.3,-1.));
#20282=CARTESIAN_POINT('',(20.,-0.3,-0.41));
#20283=CARTESIAN_POINT('',(-0.05,-0.3,-1.));
#20284=CARTESIAN_POINT('Origin',(-0.1,-0.55,-0.82));
#20285=CARTESIAN_POINT('',(0.,-0.55,-0.82));
#20286=CARTESIAN_POINT('',(0.,-0.275,-0.82));
#20287=CARTESIAN_POINT('',(20.,-0.55,-0.82));
#20288=CARTESIAN_POINT('',(-0.1,-0.55,-0.82));
#20289=CARTESIAN_POINT('',(20.,-0.275,-0.82));
#20290=CARTESIAN_POINT('Origin',(-0.1,-0.55,-0.67));
#20291=CARTESIAN_POINT('',(0.,-0.55,-0.67));
#20292=CARTESIAN_POINT('',(0.,-0.55,-0.335));
#20293=CARTESIAN_POINT('',(20.,-0.55,-0.67));
#20294=CARTESIAN_POINT('',(-0.1,-0.55,-0.67));
#20295=CARTESIAN_POINT('',(20.,-0.55,-0.335));
#20296=CARTESIAN_POINT('Origin',(-0.1,-0.3,-0.42));
#20297=CARTESIAN_POINT('',(0.,-0.3,-0.42));
#20298=CARTESIAN_POINT('',(0.,-0.12,-0.24));
#20299=CARTESIAN_POINT('',(20.,-0.3,-0.42));
#20300=CARTESIAN_POINT('',(-0.1,-0.3,-0.42));
#20301=CARTESIAN_POINT('',(20.,-0.12,-0.24));
#20302=CARTESIAN_POINT('Origin',(-0.1,0.3,-0.42));
#20303=CARTESIAN_POINT('',(0.,0.3,-0.42));
#20304=CARTESIAN_POINT('',(0.,0.15,-0.42));
#20305=CARTESIAN_POINT('',(20.,0.3,-0.42));
#20306=CARTESIAN_POINT('',(-0.1,0.3,-0.42));
#20307=CARTESIAN_POINT('',(20.,0.15,-0.42));
#20308=CARTESIAN_POINT('Origin',(-0.1,0.55,-0.67));
#20309=CARTESIAN_POINT('',(0.,0.55,-0.67));
#20310=CARTESIAN_POINT('',(0.,0.245,-0.365));
#20311=CARTESIAN_POINT('',(20.,0.55,-0.67));
#20312=CARTESIAN_POINT('',(-0.1,0.55,-0.67));
#20313=CARTESIAN_POINT('',(20.,0.245,-0.365));
#20314=CARTESIAN_POINT('Origin',(-0.1,0.55,-0.82));
#20315=CARTESIAN_POINT('',(0.,0.55,-0.82));
#20316=CARTESIAN_POINT('',(0.,0.55,-0.41));
#20317=CARTESIAN_POINT('',(20.,0.55,-0.82));
#20318=CARTESIAN_POINT('',(-0.1,0.55,-0.82));
#20319=CARTESIAN_POINT('',(20.,0.55,-0.41));
#20320=CARTESIAN_POINT('Origin',(-0.1,0.3,-0.82));
#20321=CARTESIAN_POINT('',(0.,0.3,-0.82));
#20322=CARTESIAN_POINT('',(0.,0.15,-0.82));
#20323=CARTESIAN_POINT('',(20.,0.3,-0.82));
#20324=CARTESIAN_POINT('',(-0.1,0.3,-0.82));
#20325=CARTESIAN_POINT('',(20.,0.15,-0.82));
#20326=CARTESIAN_POINT('Origin',(-0.1,0.3,-1.05));
#20327=CARTESIAN_POINT('',(0.,0.3,-1.));
#20328=CARTESIAN_POINT('',(0.,0.3,-0.525));
#20329=CARTESIAN_POINT('',(20.,0.3,-1.));
#20330=CARTESIAN_POINT('',(-0.05,0.3,-1.));
#20331=CARTESIAN_POINT('',(20.,0.3,-0.525));
#20332=CARTESIAN_POINT('Origin',(-0.1,-0.82,0.3));
#20333=CARTESIAN_POINT('',(0.,-0.82,0.3));
#20334=CARTESIAN_POINT('',(0.,-1.,0.3));
#20335=CARTESIAN_POINT('',(0.,-0.41,0.3));
#20336=CARTESIAN_POINT('',(20.,-0.82,0.3));
#20337=CARTESIAN_POINT('',(-0.1,-0.82,0.3));
#20338=CARTESIAN_POINT('',(20.,-1.,0.3));
#20339=CARTESIAN_POINT('',(20.,-0.41,0.3));
#20340=CARTESIAN_POINT('',(-0.05,-1.,0.3));
#20341=CARTESIAN_POINT('Origin',(-0.1,-0.82,0.55));
#20342=CARTESIAN_POINT('',(0.,-0.82,0.55));
#20343=CARTESIAN_POINT('',(0.,-0.82,0.275));
#20344=CARTESIAN_POINT('',(20.,-0.82,0.55));
#20345=CARTESIAN_POINT('',(-0.1,-0.82,0.55));
#20346=CARTESIAN_POINT('',(20.,-0.82,0.275));
#20347=CARTESIAN_POINT('Origin',(-0.1,-0.67,0.55));
#20348=CARTESIAN_POINT('',(0.,-0.67,0.55));
#20349=CARTESIAN_POINT('',(0.,-0.335,0.55));
#20350=CARTESIAN_POINT('',(20.,-0.67,0.55));
#20351=CARTESIAN_POINT('',(-0.1,-0.67,0.55));
#20352=CARTESIAN_POINT('',(20.,-0.335,0.55));
#20353=CARTESIAN_POINT('Origin',(-0.1,-0.42,0.3));
#20354=CARTESIAN_POINT('',(0.,-0.42,0.3));
#20355=CARTESIAN_POINT('',(-6.93889390390723E-18,-0.24,0.12));
#20356=CARTESIAN_POINT('',(20.,-0.42,0.3));
#20357=CARTESIAN_POINT('',(-0.1,-0.42,0.3));
#20358=CARTESIAN_POINT('',(20.,-0.24,0.12));
#20359=CARTESIAN_POINT('Origin',(-0.1,-0.42,-0.3));
#20360=CARTESIAN_POINT('',(0.,-0.42,-0.3));
#20361=CARTESIAN_POINT('',(0.,-0.42,-0.15));
#20362=CARTESIAN_POINT('',(20.,-0.42,-0.3));
#20363=CARTESIAN_POINT('',(-0.1,-0.42,-0.3));
#20364=CARTESIAN_POINT('',(20.,-0.42,-0.15));
#20365=CARTESIAN_POINT('Origin',(-0.1,-0.67,-0.55));
#20366=CARTESIAN_POINT('',(0.,-0.67,-0.55));
#20367=CARTESIAN_POINT('',(0.,-0.365,-0.245));
#20368=CARTESIAN_POINT('',(20.,-0.67,-0.55));
#20369=CARTESIAN_POINT('',(-0.1,-0.67,-0.55));
#20370=CARTESIAN_POINT('',(20.,-0.365,-0.245));
#20371=CARTESIAN_POINT('Origin',(-0.1,-0.82,-0.55));
#20372=CARTESIAN_POINT('',(0.,-0.82,-0.55));
#20373=CARTESIAN_POINT('',(0.,-0.41,-0.55));
#20374=CARTESIAN_POINT('',(20.,-0.82,-0.55));
#20375=CARTESIAN_POINT('',(-0.1,-0.82,-0.55));
#20376=CARTESIAN_POINT('',(20.,-0.41,-0.55));
#20377=CARTESIAN_POINT('Origin',(-0.1,-0.82,-0.3));
#20378=CARTESIAN_POINT('',(0.,-0.82,-0.3));
#20379=CARTESIAN_POINT('',(0.,-0.82,-0.15));
#20380=CARTESIAN_POINT('',(20.,-0.82,-0.3));
#20381=CARTESIAN_POINT('',(-0.1,-0.82,-0.3));
#20382=CARTESIAN_POINT('',(20.,-0.82,-0.15));
#20383=CARTESIAN_POINT('Origin',(-0.1,-1.05,-0.3));
#20384=CARTESIAN_POINT('',(0.,-1.,-0.3));
#20385=CARTESIAN_POINT('',(0.,-0.525,-0.3));
#20386=CARTESIAN_POINT('',(20.,-1.,-0.3));
#20387=CARTESIAN_POINT('',(-0.05,-1.,-0.3));
#20388=CARTESIAN_POINT('',(20.,-0.525,-0.3));
#20389=CARTESIAN_POINT('Origin',(-0.1,0.3,0.82));
#20390=CARTESIAN_POINT('',(0.,0.3,0.82));
#20391=CARTESIAN_POINT('',(0.,0.3,1.));
#20392=CARTESIAN_POINT('',(0.,0.3,0.41));
#20393=CARTESIAN_POINT('',(20.,0.3,0.82));
#20394=CARTESIAN_POINT('',(-0.1,0.3,0.82));
#20395=CARTESIAN_POINT('',(20.,0.3,1.));
#20396=CARTESIAN_POINT('',(20.,0.3,0.41));
#20397=CARTESIAN_POINT('',(-0.05,0.3,1.));
#20398=CARTESIAN_POINT('Origin',(-0.1,0.55,0.82));
#20399=CARTESIAN_POINT('',(0.,0.55,0.82));
#20400=CARTESIAN_POINT('',(0.,0.275,0.82));
#20401=CARTESIAN_POINT('',(20.,0.55,0.82));
#20402=CARTESIAN_POINT('',(-0.1,0.55,0.82));
#20403=CARTESIAN_POINT('',(20.,0.275,0.82));
#20404=CARTESIAN_POINT('Origin',(-0.1,0.55,0.67));
#20405=CARTESIAN_POINT('',(0.,0.55,0.67));
#20406=CARTESIAN_POINT('',(0.,0.55,0.335));
#20407=CARTESIAN_POINT('',(20.,0.55,0.67));
#20408=CARTESIAN_POINT('',(-0.1,0.55,0.67));
#20409=CARTESIAN_POINT('',(20.,0.55,0.335));
#20410=CARTESIAN_POINT('Origin',(-0.1,0.3,0.42));
#20411=CARTESIAN_POINT('',(0.,0.3,0.42));
#20412=CARTESIAN_POINT('',(6.93889390390723E-18,0.12,0.24));
#20413=CARTESIAN_POINT('',(20.,0.3,0.42));
#20414=CARTESIAN_POINT('',(-0.1,0.3,0.42));
#20415=CARTESIAN_POINT('',(20.,0.12,0.24));
#20416=CARTESIAN_POINT('Origin',(-0.1,-0.3,0.42));
#20417=CARTESIAN_POINT('',(0.,-0.3,0.42));
#20418=CARTESIAN_POINT('',(0.,-0.15,0.42));
#20419=CARTESIAN_POINT('',(20.,-0.3,0.42));
#20420=CARTESIAN_POINT('',(-0.1,-0.3,0.42));
#20421=CARTESIAN_POINT('',(20.,-0.15,0.42));
#20422=CARTESIAN_POINT('Origin',(-0.1,-0.55,0.67));
#20423=CARTESIAN_POINT('',(0.,-0.55,0.67));
#20424=CARTESIAN_POINT('',(6.93889390390723E-18,-0.245,0.365));
#20425=CARTESIAN_POINT('',(20.,-0.55,0.67));
#20426=CARTESIAN_POINT('',(-0.1,-0.55,0.67));
#20427=CARTESIAN_POINT('',(20.,-0.245,0.365));
#20428=CARTESIAN_POINT('Origin',(-0.1,-0.55,0.82));
#20429=CARTESIAN_POINT('',(0.,-0.55,0.82));
#20430=CARTESIAN_POINT('',(0.,-0.55,0.41));
#20431=CARTESIAN_POINT('',(20.,-0.55,0.82));
#20432=CARTESIAN_POINT('',(-0.1,-0.55,0.82));
#20433=CARTESIAN_POINT('',(20.,-0.55,0.41));
#20434=CARTESIAN_POINT('Origin',(-0.1,-0.3,0.82));
#20435=CARTESIAN_POINT('',(0.,-0.3,0.82));
#20436=CARTESIAN_POINT('',(0.,-0.15,0.82));
#20437=CARTESIAN_POINT('',(20.,-0.3,0.82));
#20438=CARTESIAN_POINT('',(-0.1,-0.3,0.82));
#20439=CARTESIAN_POINT('',(20.,-0.15,0.82));
#20440=CARTESIAN_POINT('Origin',(-0.1,-0.3,1.05));
#20441=CARTESIAN_POINT('',(0.,-0.3,1.));
#20442=CARTESIAN_POINT('',(0.,-0.3,0.525));
#20443=CARTESIAN_POINT('',(20.,-0.3,1.));
#20444=CARTESIAN_POINT('',(-0.05,-0.3,1.));
#20445=CARTESIAN_POINT('',(20.,-0.3,0.525));
#20446=CARTESIAN_POINT('Origin',(-0.1,0.,0.));
#20447=CARTESIAN_POINT('',(0.,-2.57175827820944E-17,0.21));
#20448=CARTESIAN_POINT('Origin',(0.,0.,0.));
#20449=CARTESIAN_POINT('',(20.,2.57175827820944E-17,0.21));
#20450=CARTESIAN_POINT('',(-0.1,-2.57175827820944E-17,0.21));
#20451=CARTESIAN_POINT('Origin',(20.,0.,0.));
#20452=CARTESIAN_POINT('Origin',(0.,1.,-1.));
#20453=CARTESIAN_POINT('',(0.,1.,1.));
#20454=CARTESIAN_POINT('',(0.,1.,-1.));
#20455=CARTESIAN_POINT('',(20.,1.,1.));
#20456=CARTESIAN_POINT('',(0.,1.,1.));
#20457=CARTESIAN_POINT('',(20.,1.,-1.));
#20458=CARTESIAN_POINT('Origin',(0.,1.,-1.));
#20459=CARTESIAN_POINT('',(20.,1.,-1.));
#20460=CARTESIAN_POINT('',(20.,1.,-1.));
#20461=CARTESIAN_POINT('',(0.,1.,-1.));
#20462=CARTESIAN_POINT('',(0.,1.,-1.));
#20463=CARTESIAN_POINT('',(0.,1.,-1.));
#20464=CARTESIAN_POINT('Origin',(0.,-1.,-1.));
#20465=CARTESIAN_POINT('',(0.,-1.,-1.));
#20466=CARTESIAN_POINT('',(20.,-1.,-1.));
#20467=CARTESIAN_POINT('Origin',(0.,-1.,-1.));
#20468=CARTESIAN_POINT('',(20.,-1.,-1.));
#20469=CARTESIAN_POINT('',(20.,-1.,-1.));
#20470=CARTESIAN_POINT('',(0.,-1.,-1.));
#20471=CARTESIAN_POINT('',(0.,-1.,-1.));
#20472=CARTESIAN_POINT('',(0.,-1.,-1.));
#20473=CARTESIAN_POINT('Origin',(0.,-1.,1.));
#20474=CARTESIAN_POINT('',(0.,-1.,1.));
#20475=CARTESIAN_POINT('',(20.,-1.,1.));
#20476=CARTESIAN_POINT('Origin',(0.,-1.,1.));
#20477=CARTESIAN_POINT('',(20.,-1.,1.));
#20478=CARTESIAN_POINT('',(20.,-1.,1.));
#20479=CARTESIAN_POINT('',(0.,-1.,1.));
#20480=CARTESIAN_POINT('',(0.,-1.,1.));
#20481=CARTESIAN_POINT('',(0.,-1.,1.));
#20482=CARTESIAN_POINT('Origin',(0.,1.,1.));
#20483=CARTESIAN_POINT('',(0.,1.,1.));
#20484=CARTESIAN_POINT('',(20.,1.,1.));
#20485=CARTESIAN_POINT('Origin',(0.,1.,1.));
#20486=CARTESIAN_POINT('',(20.,1.,1.));
#20487=CARTESIAN_POINT('',(0.,1.,1.));
#20488=CARTESIAN_POINT('Origin',(20.,0.,0.));
#20489=CARTESIAN_POINT('Origin',(0.,0.,0.));
#20490=CARTESIAN_POINT('',(0.,0.,0.));
#20491=CARTESIAN_POINT('Origin',(0.,0.395,0.25));
#20492=CARTESIAN_POINT('',(-0.5,0.3,0.25));
#20493=CARTESIAN_POINT('',(0.5,0.3,0.25));
#20494=CARTESIAN_POINT('',(0.25,0.3,0.25));
#20495=CARTESIAN_POINT('',(-0.5,0.5,0.25));
#20496=CARTESIAN_POINT('',(-0.5,0.5,0.25));
#20497=CARTESIAN_POINT('',(0.5,0.5,0.25));
#20498=CARTESIAN_POINT('',(0.5,0.5,0.25));
#20499=CARTESIAN_POINT('',(0.5,0.29,0.25));
#20500=CARTESIAN_POINT('Origin',(0.5,0.5,0.25));
#20501=CARTESIAN_POINT('',(-0.5,0.5,0.4));
#20502=CARTESIAN_POINT('',(-0.5,0.5,0.25));
#20503=CARTESIAN_POINT('',(0.5,0.5,0.4));
#20504=CARTESIAN_POINT('',(0.5,0.5,0.4));
#20505=CARTESIAN_POINT('',(0.5,0.5,0.25));
#20506=CARTESIAN_POINT('Origin',(0.,0.,0.4));
#20507=CARTESIAN_POINT('',(-0.5,-0.5,0.4));
#20508=CARTESIAN_POINT('',(-0.5,0.5,0.4));
#20509=CARTESIAN_POINT('',(0.5,-0.5,0.4));
#20510=CARTESIAN_POINT('',(-0.5,-0.5,0.4));
#20511=CARTESIAN_POINT('',(0.5,-0.3,0.4));
#20512=CARTESIAN_POINT('',(-0.2117,2.59257727379495E-17,0.4));
#20513=CARTESIAN_POINT('Origin',(0.,0.,0.4));
#20514=CARTESIAN_POINT('Origin',(-0.5,0.3,0.));
#20515=CARTESIAN_POINT('',(-0.5,0.3,0.15));
#20516=CARTESIAN_POINT('',(-0.5,0.3,0.));
#20517=CARTESIAN_POINT('',(-0.5,0.15,0.));
#20518=CARTESIAN_POINT('',(-0.5,0.225,0.075));
#20519=CARTESIAN_POINT('',(-0.5,-0.15,0.));
#20520=CARTESIAN_POINT('',(-0.5,0.3,0.));
#20521=CARTESIAN_POINT('',(-0.5,-0.3,0.15));
#20522=CARTESIAN_POINT('',(-0.5,-0.075,-0.075));
#20523=CARTESIAN_POINT('',(-0.5,-0.3,0.25));
#20524=CARTESIAN_POINT('',(-0.5,-0.3,0.));
#20525=CARTESIAN_POINT('',(-0.5,-0.5,0.25));
#20526=CARTESIAN_POINT('',(-0.5,-0.29,0.25));
#20527=CARTESIAN_POINT('',(-0.5,-0.5,0.25));
#20528=CARTESIAN_POINT('Origin',(-0.5,-0.5,0.25));
#20529=CARTESIAN_POINT('',(0.5,-0.5,0.25));
#20530=CARTESIAN_POINT('',(-0.5,-0.5,0.25));
#20531=CARTESIAN_POINT('',(0.5,-0.5,0.25));
#20532=CARTESIAN_POINT('Origin',(0.,-0.395,0.25));
#20533=CARTESIAN_POINT('',(0.5,-0.3,0.25));
#20534=CARTESIAN_POINT('',(-0.25,-0.3,0.25));
#20535=CARTESIAN_POINT('',(0.5,-0.5,0.25));
#20536=CARTESIAN_POINT('Origin',(0.5,-0.3,0.));
#20537=CARTESIAN_POINT('',(0.5,-0.3,0.15));
#20538=CARTESIAN_POINT('',(0.5,-0.3,0.));
#20539=CARTESIAN_POINT('',(0.5,-0.15,0.));
#20540=CARTESIAN_POINT('',(0.5,-0.225,0.075));
#20541=CARTESIAN_POINT('',(0.5,0.15,0.));
#20542=CARTESIAN_POINT('',(0.5,-0.3,0.));
#20543=CARTESIAN_POINT('',(0.5,0.3,0.15));
#20544=CARTESIAN_POINT('',(0.5,0.075,-0.075));
#20545=CARTESIAN_POINT('',(0.5,0.3,0.));
#20546=CARTESIAN_POINT('Origin',(-0.5,-0.3,0.));
#20547=CARTESIAN_POINT('',(-0.25,-0.3,0.15));
#20548=CARTESIAN_POINT('Origin',(-0.25,-0.225,0.075));
#20549=CARTESIAN_POINT('',(-0.149388386429468,-0.15,0.));
#20550=CARTESIAN_POINT('',(-0.25,-0.15,0.));
#20551=CARTESIAN_POINT('',(0.149388386429468,-0.15,0.));
#20552=CARTESIAN_POINT('Origin',(0.,0.,-0.15));
#20553=CARTESIAN_POINT('',(-0.25,-0.15,0.));
#20554=CARTESIAN_POINT('Origin',(0.,0.,-0.1));
#20555=CARTESIAN_POINT('',(-0.2117,-2.59257727379495E-17,0.));
#20556=CARTESIAN_POINT('Origin',(0.,0.,0.));
#20557=CARTESIAN_POINT('',(-0.2117,-2.59257727379495E-17,-0.1));
#20558=CARTESIAN_POINT('',(-0.149388386429468,0.15,0.));
#20559=CARTESIAN_POINT('Origin',(0.,0.,0.));
#20560=CARTESIAN_POINT('',(0.149388386429468,0.15,0.));
#20561=CARTESIAN_POINT('Origin',(0.,0.,-0.15));
#20562=CARTESIAN_POINT('Origin',(0.,0.,0.));
#20563=CARTESIAN_POINT('Origin',(0.,0.,0.));
#20564=CARTESIAN_POINT('',(0.25,0.15,0.));
#20565=CARTESIAN_POINT('Origin',(0.,0.,0.));
#20566=CARTESIAN_POINT('',(0.25,0.15,0.));
#20567=CARTESIAN_POINT('Origin',(0.25,0.225,0.075));
#20568=CARTESIAN_POINT('',(0.25,0.3,0.15));
#20569=CARTESIAN_POINT('Origin',(0.5,0.3,0.));
#20570=CARTESIAN_POINT('',(0.,0.,0.));
#20571=CARTESIAN_POINT('Origin',(0.,0.09,0.));
#20572=CARTESIAN_POINT('',(-0.285,0.1,3.49024337756996E-17));
#20573=CARTESIAN_POINT('Origin',(0.,0.1,0.));
#20574=CARTESIAN_POINT('',(-0.265,0.08,-3.24531401774049E-17));
#20575=CARTESIAN_POINT('',(-0.275,0.09,3.36777869765522E-17));
#20576=CARTESIAN_POINT('Origin',(0.,0.08,0.));
#20577=CARTESIAN_POINT('Origin',(0.,0.,0.));
#20578=CARTESIAN_POINT('',(-0.265,0.,3.24531401774049E-17));
#20579=CARTESIAN_POINT('',(-0.265,0.,3.24531401774049E-17));
#20580=CARTESIAN_POINT('Origin',(0.,0.,0.));
#20581=CARTESIAN_POINT('Origin',(0.,0.1,0.));
#20582=CARTESIAN_POINT('',(-0.5,0.1,6.12323399573677E-17));
#20583=CARTESIAN_POINT('Origin',(0.,0.1,0.));
#20584=CARTESIAN_POINT('Origin',(0.,0.,0.));
#20585=CARTESIAN_POINT('',(-0.5,0.,6.12323399573677E-17));
#20586=CARTESIAN_POINT('',(-0.5,0.,6.12323399573677E-17));
#20587=CARTESIAN_POINT('Origin',(0.,0.,0.));
#20588=CARTESIAN_POINT('Origin',(0.,0.,0.));
#20589=CARTESIAN_POINT('',(0.,0.,0.));
#20590=CARTESIAN_POINT('Origin',(14.,0.,0.97));
#20591=CARTESIAN_POINT('',(13.625,-4.59242549680257E-17,0.97));
#20592=CARTESIAN_POINT('Origin',(14.,0.,0.97));
#20593=CARTESIAN_POINT('',(13.625,4.59242549680257E-17,1.5));
#20594=CARTESIAN_POINT('',(13.625,-4.59242549680257E-17,0.97));
#20595=CARTESIAN_POINT('Origin',(14.,0.,1.5));
#20596=CARTESIAN_POINT('Origin',(14.,0.,0.97));
#20597=CARTESIAN_POINT('',(13.775,-2.75545529808154E-17,0.97));
#20598=CARTESIAN_POINT('Origin',(14.,0.,0.97));
#20599=CARTESIAN_POINT('Origin',(8.,0.,0.97));
#20600=CARTESIAN_POINT('',(7.625,-4.59242549680257E-17,0.97));
#20601=CARTESIAN_POINT('Origin',(8.,0.,0.97));
#20602=CARTESIAN_POINT('',(7.625,4.59242549680257E-17,1.5));
#20603=CARTESIAN_POINT('',(7.625,-4.59242549680257E-17,0.97));
#20604=CARTESIAN_POINT('Origin',(8.,0.,1.5));
#20605=CARTESIAN_POINT('Origin',(8.,0.,0.97));
#20606=CARTESIAN_POINT('',(7.775,-2.75545529808154E-17,0.97));
#20607=CARTESIAN_POINT('Origin',(8.,0.,0.97));
#20608=CARTESIAN_POINT('Origin',(2.,0.,0.97));
#20609=CARTESIAN_POINT('',(1.625,-4.59242549680257E-17,0.97));
#20610=CARTESIAN_POINT('Origin',(2.,0.,0.97));
#20611=CARTESIAN_POINT('',(1.625,4.59242549680257E-17,1.5));
#20612=CARTESIAN_POINT('',(1.625,-4.59242549680257E-17,0.97));
#20613=CARTESIAN_POINT('Origin',(2.,0.,1.5));
#20614=CARTESIAN_POINT('Origin',(2.,0.,0.97));
#20615=CARTESIAN_POINT('',(1.775,-2.75545529808155E-17,0.97));
#20616=CARTESIAN_POINT('Origin',(2.,0.,0.97));
#20617=CARTESIAN_POINT('Origin',(20.,0.,0.97));
#20618=CARTESIAN_POINT('',(19.625,-4.59242549680257E-17,0.97));
#20619=CARTESIAN_POINT('Origin',(20.,0.,0.97));
#20620=CARTESIAN_POINT('',(19.625,4.59242549680257E-17,1.5));
#20621=CARTESIAN_POINT('',(19.625,-4.59242549680257E-17,0.97));
#20622=CARTESIAN_POINT('Origin',(20.,0.,1.5));
#20623=CARTESIAN_POINT('Origin',(20.,0.,0.97));
#20624=CARTESIAN_POINT('',(19.775,-2.75545529808156E-17,0.97));
#20625=CARTESIAN_POINT('Origin',(20.,0.,0.97));
#20626=CARTESIAN_POINT('Origin',(14.,0.,-0.1));
#20627=CARTESIAN_POINT('',(13.775,-2.75545529808154E-17,0.));
#20628=CARTESIAN_POINT('Origin',(14.,0.,0.));
#20629=CARTESIAN_POINT('',(13.775,-2.75545529808154E-17,-0.1));
#20630=CARTESIAN_POINT('Origin',(8.,0.,-0.1));
#20631=CARTESIAN_POINT('',(7.775,-2.75545529808154E-17,0.));
#20632=CARTESIAN_POINT('Origin',(8.,0.,0.));
#20633=CARTESIAN_POINT('',(7.775,-2.75545529808154E-17,-0.1));
#20634=CARTESIAN_POINT('Origin',(2.,0.,-0.1));
#20635=CARTESIAN_POINT('',(1.775,-2.75545529808155E-17,0.));
#20636=CARTESIAN_POINT('Origin',(2.,0.,0.));
#20637=CARTESIAN_POINT('',(1.775,-2.75545529808155E-17,-0.1));
#20638=CARTESIAN_POINT('Origin',(20.,0.,-0.1));
#20639=CARTESIAN_POINT('',(19.775,-2.75545529808156E-17,0.));
#20640=CARTESIAN_POINT('Origin',(20.,0.,0.));
#20641=CARTESIAN_POINT('',(19.775,-2.75545529808156E-17,-0.1));
#20642=CARTESIAN_POINT('Origin',(0.,-0.53,1.));
#20643=CARTESIAN_POINT('',(0.,-0.53,1.));
#20644=CARTESIAN_POINT('',(0.,-0.75,0.85));
#20645=CARTESIAN_POINT('',(0.,-0.53,1.));
#20646=CARTESIAN_POINT('',(22.,-0.75,0.85));
#20647=CARTESIAN_POINT('',(0.,-0.75,0.85));
#20648=CARTESIAN_POINT('',(22.,-0.53,1.));
#20649=CARTESIAN_POINT('',(22.,-0.53,1.));
#20650=CARTESIAN_POINT('',(0.,-0.53,1.));
#20651=CARTESIAN_POINT('Origin',(0.,-0.53,1.15));
#20652=CARTESIAN_POINT('',(0.,-0.53,1.15));
#20653=CARTESIAN_POINT('',(0.,-0.53,1.15));
#20654=CARTESIAN_POINT('',(22.,-0.53,1.15));
#20655=CARTESIAN_POINT('',(22.,-0.53,1.15));
#20656=CARTESIAN_POINT('',(0.,-0.53,1.15));
#20657=CARTESIAN_POINT('Origin',(0.,-0.75,1.3));
#20658=CARTESIAN_POINT('',(0.,-0.75,1.3));
#20659=CARTESIAN_POINT('',(0.,-0.75,1.3));
#20660=CARTESIAN_POINT('',(22.,-0.75,1.3));
#20661=CARTESIAN_POINT('',(22.,-0.75,1.3));
#20662=CARTESIAN_POINT('',(0.,-0.75,1.3));
#20663=CARTESIAN_POINT('Origin',(0.,-0.75,1.5));
#20664=CARTESIAN_POINT('',(0.,-0.75,1.5));
#20665=CARTESIAN_POINT('',(0.,-0.75,1.5));
#20666=CARTESIAN_POINT('',(22.,-0.75,1.5));
#20667=CARTESIAN_POINT('',(22.,-0.75,1.5));
#20668=CARTESIAN_POINT('',(0.,-0.75,1.5));
#20669=CARTESIAN_POINT('Origin',(0.,0.75,1.5));
#20670=CARTESIAN_POINT('',(0.,0.75,1.5));
#20671=CARTESIAN_POINT('',(0.,0.75,1.5));
#20672=CARTESIAN_POINT('',(22.,0.75,1.5));
#20673=CARTESIAN_POINT('',(22.,0.75,1.5));
#20674=CARTESIAN_POINT('',(0.,0.75,1.5));
#20675=CARTESIAN_POINT('Origin',(0.,0.75,1.3));
#20676=CARTESIAN_POINT('',(0.,0.75,1.3));
#20677=CARTESIAN_POINT('',(0.,0.75,1.3));
#20678=CARTESIAN_POINT('',(22.,0.75,1.3));
#20679=CARTESIAN_POINT('',(22.,0.75,1.3));
#20680=CARTESIAN_POINT('',(0.,0.75,1.3));
#20681=CARTESIAN_POINT('Origin',(0.,0.53,1.15));
#20682=CARTESIAN_POINT('',(0.,0.53,1.15));
#20683=CARTESIAN_POINT('',(0.,0.53,1.15));
#20684=CARTESIAN_POINT('',(22.,0.53,1.15));
#20685=CARTESIAN_POINT('',(22.,0.53,1.15));
#20686=CARTESIAN_POINT('',(0.,0.53,1.15));
#20687=CARTESIAN_POINT('Origin',(0.,0.53,1.));
#20688=CARTESIAN_POINT('',(0.,0.53,1.));
#20689=CARTESIAN_POINT('',(0.,0.53,1.));
#20690=CARTESIAN_POINT('',(22.,0.53,1.));
#20691=CARTESIAN_POINT('',(22.,0.53,1.));
#20692=CARTESIAN_POINT('',(0.,0.53,1.));
#20693=CARTESIAN_POINT('Origin',(0.,0.75,0.85));
#20694=CARTESIAN_POINT('',(0.,0.75,0.85));
#20695=CARTESIAN_POINT('',(0.,0.75,0.85));
#20696=CARTESIAN_POINT('',(22.,0.75,0.85));
#20697=CARTESIAN_POINT('',(22.,0.75,0.85));
#20698=CARTESIAN_POINT('',(0.,0.75,0.85));
#20699=CARTESIAN_POINT('Origin',(0.,0.75,0.));
#20700=CARTESIAN_POINT('',(0.,0.75,0.));
#20701=CARTESIAN_POINT('',(0.,0.75,0.));
#20702=CARTESIAN_POINT('',(22.,0.75,0.));
#20703=CARTESIAN_POINT('',(22.,0.75,0.));
#20704=CARTESIAN_POINT('',(0.,0.75,0.));
#20705=CARTESIAN_POINT('Origin',(0.,-0.75,0.));
#20706=CARTESIAN_POINT('',(0.,-0.75,0.));
#20707=CARTESIAN_POINT('',(0.,-0.75,0.));
#20708=CARTESIAN_POINT('',(22.,-0.75,0.));
#20709=CARTESIAN_POINT('',(22.,-0.75,0.));
#20710=CARTESIAN_POINT('',(0.,-0.75,0.));
#20711=CARTESIAN_POINT('Origin',(0.,-0.75,0.85));
#20712=CARTESIAN_POINT('',(0.,-0.75,0.85));
#20713=CARTESIAN_POINT('',(22.,-0.75,0.85));
#20714=CARTESIAN_POINT('Origin',(22.,0.,0.75));
#20715=CARTESIAN_POINT('Origin',(0.,0.,0.75));
#20716=CARTESIAN_POINT('',(0.,0.,0.));
#20717=CARTESIAN_POINT('Origin',(0.375,0.5,0.));
#20718=CARTESIAN_POINT('',(-0.375,0.5,-4.59242549680257E-17));
#20719=CARTESIAN_POINT('Origin',(0.,0.5,0.));
#20720=CARTESIAN_POINT('Origin',(0.,0.475,0.));
#20721=CARTESIAN_POINT('',(-0.425,0.45,-5.20474889637625E-17));
#20722=CARTESIAN_POINT('Origin',(0.,0.45,0.));
#20723=CARTESIAN_POINT('',(-0.4,0.475,-4.89858719658941E-17));
#20724=CARTESIAN_POINT('Origin',(0.,0.24,0.));
#20725=CARTESIAN_POINT('',(-0.425,0.0299999999999998,-5.20474889637625E-17));
#20726=CARTESIAN_POINT('Origin',(0.,0.0299999999999998,0.));
#20727=CARTESIAN_POINT('',(-0.425,0.24,-5.20474889637625E-17));
#20728=CARTESIAN_POINT('Origin',(0.,0.0150000000000001,0.));
#20729=CARTESIAN_POINT('',(-0.395,4.85722573273506E-17,-4.83735485663204E-17));
#20730=CARTESIAN_POINT('Origin',(0.,0.,0.));
#20731=CARTESIAN_POINT('',(-0.41,0.0150000000000001,-5.02105187650415E-17));
#20732=CARTESIAN_POINT('Origin',(0.27,0.,0.));
#20733=CARTESIAN_POINT('',(-0.27,0.,-3.30654635769785E-17));
#20734=CARTESIAN_POINT('Origin',(0.,0.,0.));
#20735=CARTESIAN_POINT('Origin',(0.,-0.02,0.));
#20736=CARTESIAN_POINT('',(-0.24505,-0.0498999999999999,3.00099698131059E-17));
#20737=CARTESIAN_POINT('Origin',(0.,-0.0498999999999999,0.));
#20738=CARTESIAN_POINT('',(-0.26,-0.02,-3.18408167778312E-17));
#20739=CARTESIAN_POINT('Origin',(0.,-0.995,0.));
#20740=CARTESIAN_POINT('',(-0.24505,-1.95495,3.00099698131059E-17));
#20741=CARTESIAN_POINT('Origin',(0.,-1.95495,0.));
#20742=CARTESIAN_POINT('',(-0.24505,-0.995,-3.00099698131059E-17));
#20743=CARTESIAN_POINT('Origin',(0.,-1.975,0.));
#20744=CARTESIAN_POINT('',(-0.2,-2.,-2.44929359829471E-17));
#20745=CARTESIAN_POINT('Origin',(0.,-2.,0.));
#20746=CARTESIAN_POINT('',(-0.225,-1.975,-2.75545529808154E-17));
#20747=CARTESIAN_POINT('Origin',(0.,-2.,0.));
#20748=CARTESIAN_POINT('Origin',(0.115470053837925,-0.5,-0.2));
#20749=CARTESIAN_POINT('',(0.23094010767585,-0.5,0.));
#20750=CARTESIAN_POINT('',(0.115470053837925,-0.5,-0.2));
#20751=CARTESIAN_POINT('',(0.23094010767585,-0.5,0.));
#20752=CARTESIAN_POINT('',(0.115470053837925,-0.8,-0.2));
#20753=CARTESIAN_POINT('',(0.115470053837925,-0.5,-0.2));
#20754=CARTESIAN_POINT('',(0.23094010767585,-0.8,0.));
#20755=CARTESIAN_POINT('',(0.23094010767585,-0.8,0.));
#20756=CARTESIAN_POINT('',(0.23094010767585,-0.5,0.));
#20757=CARTESIAN_POINT('Origin',(-0.115470053837925,-0.5,-0.2));
#20758=CARTESIAN_POINT('',(-0.115470053837925,-0.5,-0.2));
#20759=CARTESIAN_POINT('',(0.115470053837925,-0.5,-0.2));
#20760=CARTESIAN_POINT('',(-0.115470053837925,-0.8,-0.2));
#20761=CARTESIAN_POINT('',(-0.115470053837925,-0.5,-0.2));
#20762=CARTESIAN_POINT('',(0.115470053837925,-0.8,-0.2));
#20763=CARTESIAN_POINT('Origin',(-0.23094010767585,-0.5,-2.77555756156289E-17));
#20764=CARTESIAN_POINT('',(-0.23094010767585,-0.5,-2.82820063659975E-17));
#20765=CARTESIAN_POINT('',(-0.115470053837925,-0.5,-0.2));
#20766=CARTESIAN_POINT('',(-0.23094010767585,-0.8,-2.77555756156289E-17));
#20767=CARTESIAN_POINT('',(-0.23094010767585,-0.5,-2.82820063659975E-17));
#20768=CARTESIAN_POINT('',(-0.115470053837925,-0.8,-0.2));
#20769=CARTESIAN_POINT('Origin',(-0.115470053837925,-0.5,0.2));
#20770=CARTESIAN_POINT('',(-0.115470053837925,-0.5,0.2));
#20771=CARTESIAN_POINT('',(-0.23094010767585,-0.5,-2.82820063659975E-17));
#20772=CARTESIAN_POINT('',(-0.115470053837925,-0.8,0.2));
#20773=CARTESIAN_POINT('',(-0.115470053837925,-0.5,0.2));
#20774=CARTESIAN_POINT('',(-0.23094010767585,-0.8,-2.82820063659975E-17));
#20775=CARTESIAN_POINT('Origin',(0.115470053837925,-0.5,0.2));
#20776=CARTESIAN_POINT('',(0.115470053837925,-0.5,0.2));
#20777=CARTESIAN_POINT('',(-0.115470053837925,-0.5,0.2));
#20778=CARTESIAN_POINT('',(0.115470053837925,-0.8,0.2));
#20779=CARTESIAN_POINT('',(0.115470053837925,-0.5,0.2));
#20780=CARTESIAN_POINT('',(-0.115470053837925,-0.8,0.2));
#20781=CARTESIAN_POINT('Origin',(0.23094010767585,-0.5,0.));
#20782=CARTESIAN_POINT('',(0.115470053837925,-0.5,0.2));
#20783=CARTESIAN_POINT('',(0.115470053837925,-0.8,0.2));
#20784=CARTESIAN_POINT('Origin',(0.,-0.5,0.));
#20785=CARTESIAN_POINT('Origin',(0.,-0.8,0.));
#20786=CARTESIAN_POINT('',(0.,0.,0.));
#20787=CARTESIAN_POINT('',(0.,0.,0.));
#20788=CARTESIAN_POINT('Origin',(0.,0.,0.));
#20789=CARTESIAN_POINT('',(-1.070235,-0.308121667383195,-1.31065986708547E-16));
#20790=CARTESIAN_POINT('',(-1.31065986708547E-16,-0.308121667383195,1.070235));
#20791=CARTESIAN_POINT('Origin',(0.,-0.308121667383195,0.));
#20792=CARTESIAN_POINT('Origin',(0.,-0.308121667383195,0.));
#20793=CARTESIAN_POINT('',(-1.31065986708547E-16,0.308121667383195,1.070235));
#20794=CARTESIAN_POINT('Origin',(-1.34711147906209E-16,0.,1.1));
#20795=CARTESIAN_POINT('',(-1.070235,0.308121667383195,1.31065986708547E-16));
#20796=CARTESIAN_POINT('Origin',(0.,0.308121667383195,0.));
#20797=CARTESIAN_POINT('Origin',(0.,0.308121667383195,0.));
#20798=CARTESIAN_POINT('Origin',(0.,0.,0.));
#20799=CARTESIAN_POINT('',(-1.070235,0.5,-1.31065986708547E-16));
#20800=CARTESIAN_POINT('',(-1.070235,0.,-1.31065986708547E-16));
#20801=CARTESIAN_POINT('Origin',(0.,0.5,0.));
#20802=CARTESIAN_POINT('Origin',(0.,0.,0.));
#20803=CARTESIAN_POINT('',(-0.6,-0.44,-7.34788079488412E-17));
#20804=CARTESIAN_POINT('Origin',(0.,-0.44,0.));
#20805=CARTESIAN_POINT('',(-0.6,0.44,-7.34788079488412E-17));
#20806=CARTESIAN_POINT('',(-0.6,0.,-7.34788079488412E-17));
#20807=CARTESIAN_POINT('Origin',(0.,0.44,0.));
#20808=CARTESIAN_POINT('Origin',(0.,0.47,0.));
#20809=CARTESIAN_POINT('',(-0.66,0.5,-8.08266887437253E-17));
#20810=CARTESIAN_POINT('',(-0.63,0.47,-7.71527483462832E-17));
#20811=CARTESIAN_POINT('Origin',(0.,0.5,0.));
#20812=CARTESIAN_POINT('Origin',(1.070235,0.5,0.));
#20813=CARTESIAN_POINT('Origin',(0.,0.,0.));
#20814=CARTESIAN_POINT('',(-1.070235,-0.5,-1.31065986708547E-16));
#20815=CARTESIAN_POINT('Origin',(0.,-0.5,0.));
#20816=CARTESIAN_POINT('',(-1.070235,0.,-1.31065986708547E-16));
#20817=CARTESIAN_POINT('Origin',(0.66,-0.5,0.));
#20818=CARTESIAN_POINT('',(-0.66,-0.5,-8.08266887437253E-17));
#20819=CARTESIAN_POINT('Origin',(0.,-0.5,0.));
#20820=CARTESIAN_POINT('Origin',(0.,-0.47,0.));
#20821=CARTESIAN_POINT('',(-0.63,-0.47,-7.71527483462832E-17));
#20822=CARTESIAN_POINT('',(0.,0.,0.));
#20823=CARTESIAN_POINT('Origin',(0.,0.,0.));
#20824=CARTESIAN_POINT('',(-1.129765,0.308121667383195,-1.38356309103871E-16));
#20825=CARTESIAN_POINT('',(-1.38356309103871E-16,0.308121667383195,1.129765));
#20826=CARTESIAN_POINT('Origin',(0.,0.308121667383195,0.));
#20827=CARTESIAN_POINT('Origin',(0.,0.308121667383195,0.));
#20828=CARTESIAN_POINT('',(-1.38356309103871E-16,-0.308121667383195,1.129765));
#20829=CARTESIAN_POINT('Origin',(-1.34711147906209E-16,0.,1.1));
#20830=CARTESIAN_POINT('',(-1.129765,-0.308121667383195,1.38356309103871E-16));
#20831=CARTESIAN_POINT('Origin',(0.,-0.308121667383195,0.));
#20832=CARTESIAN_POINT('Origin',(0.,-0.308121667383195,0.));
#20833=CARTESIAN_POINT('Origin',(0.,0.,0.));
#20834=CARTESIAN_POINT('',(-1.129765,-0.5,-1.38356309103871E-16));
#20835=CARTESIAN_POINT('Origin',(0.,-0.5,0.));
#20836=CARTESIAN_POINT('',(-1.129765,0.,-1.38356309103871E-16));
#20837=CARTESIAN_POINT('Origin',(1.54,0.5,0.));
#20838=CARTESIAN_POINT('',(-1.54,0.5,-1.88595607068692E-16));
#20839=CARTESIAN_POINT('Origin',(0.,0.5,0.));
#20840=CARTESIAN_POINT('',(-1.129765,0.5,-1.38356309103871E-16));
#20841=CARTESIAN_POINT('Origin',(0.,0.5,0.));
#20842=CARTESIAN_POINT('Origin',(0.,0.47,0.));
#20843=CARTESIAN_POINT('',(-1.6,0.44,-1.95943487863577E-16));
#20844=CARTESIAN_POINT('Origin',(0.,0.44,0.));
#20845=CARTESIAN_POINT('',(-1.57,0.47,-1.92269547466134E-16));
#20846=CARTESIAN_POINT('Origin',(0.,0.,0.));
#20847=CARTESIAN_POINT('',(-1.6,-0.44,-1.95943487863577E-16));
#20848=CARTESIAN_POINT('Origin',(0.,-0.44,0.));
#20849=CARTESIAN_POINT('',(-1.6,0.,-1.95943487863577E-16));
#20850=CARTESIAN_POINT('Origin',(0.,-0.47,0.));
#20851=CARTESIAN_POINT('',(-1.54,-0.5,-1.88595607068692E-16));
#20852=CARTESIAN_POINT('Origin',(0.,-0.5,0.));
#20853=CARTESIAN_POINT('',(-1.57,-0.47,-1.92269547466134E-16));
#20854=CARTESIAN_POINT('Origin',(1.129765,-0.5,0.));
#20855=CARTESIAN_POINT('Origin',(0.,0.,0.));
#20856=CARTESIAN_POINT('',(-1.129765,0.,-1.38356309103871E-16));
#20857=CARTESIAN_POINT('',(0.,0.,0.));
#20858=CARTESIAN_POINT('Origin',(1.1,0.,0.));
#20859=CARTESIAN_POINT('',(1.1,-2.23201749654651E-33,0.29765));
#20860=CARTESIAN_POINT('',(1.1,-2.23201749654651E-33,-0.29765));
#20861=CARTESIAN_POINT('Origin',(1.1,0.,0.));
#20862=CARTESIAN_POINT('Origin',(0.685838782044607,0.,-0.860014630714833));
#20863=CARTESIAN_POINT('',(0.918550922801216,-5.31350540756609E-33,-0.674432891191581));
#20864=CARTESIAN_POINT('',(0.453126641287998,8.49470414473068E-34,-1.04559637023808));
#20865=CARTESIAN_POINT('Origin',(0.685838782044607,0.,-0.860014630714833));
#20866=CARTESIAN_POINT('Origin',(-0.244773027351946,0.,-1.07242070340001));
#20867=CARTESIAN_POINT('',(0.0454142657089739,-2.23201749654651E-33,-1.1386540593921));
#20868=CARTESIAN_POINT('',(-0.534960320412865,-2.23201749654651E-33,-1.00618734740791));
#20869=CARTESIAN_POINT('Origin',(-0.244773027351946,0.,-1.07242070340001));
#20870=CARTESIAN_POINT('Origin',(-0.991065754692661,0.,-0.477272113029314));
#20871=CARTESIAN_POINT('',(-0.86192025974432,8.49470414473067E-34,-0.745445496560469));
#20872=CARTESIAN_POINT('',(-1.120211249641,-5.31350540756609E-33,-0.209098729498159));
#20873=CARTESIAN_POINT('Origin',(-0.991065754692661,0.,-0.477272113029314));
#20874=CARTESIAN_POINT('Origin',(-0.991065754692661,0.,0.477272113029314));
#20875=CARTESIAN_POINT('',(-1.120211249641,-2.23201749654651E-33,0.209098729498159));
#20876=CARTESIAN_POINT('',(-0.86192025974432,-2.23201749654651E-33,0.745445496560469));
#20877=CARTESIAN_POINT('Origin',(-0.991065754692661,0.,0.477272113029314));
#20878=CARTESIAN_POINT('Origin',(-0.244773027351946,0.,1.07242070340001));
#20879=CARTESIAN_POINT('',(-0.534960320412866,-2.23201749654651E-33,1.00618734740791));
#20880=CARTESIAN_POINT('',(0.0454142657089737,-2.23201749654651E-33,1.1386540593921));
#20881=CARTESIAN_POINT('Origin',(-0.244773027351946,0.,1.07242070340001));
#20882=CARTESIAN_POINT('Origin',(0.685838782044607,0.,0.860014630714833));
#20883=CARTESIAN_POINT('',(0.453126641287998,-2.23201749654651E-33,1.04559637023808));
#20884=CARTESIAN_POINT('',(0.918550922801216,-2.23201749654651E-33,0.674432891191581));
#20885=CARTESIAN_POINT('Origin',(0.685838782044607,0.,0.860014630714833));
#20886=CARTESIAN_POINT('',(0.,0.,0.));
#20887=CARTESIAN_POINT('Origin',(0.685838782044607,0.,0.860014630714833));
#20888=CARTESIAN_POINT('',(0.413083465285518,-0.05953,0.993751811093549));
#20889=CARTESIAN_POINT('',(0.876916659919095,-0.05953,0.623857181492959));
#20890=CARTESIAN_POINT('Ctrl Pts',(0.413083465285518,-0.05953,0.993751811093549));
#20891=CARTESIAN_POINT('Ctrl Pts',(0.419070565453383,-0.0925528133349865,
0.991263089003441));
#20892=CARTESIAN_POINT('Ctrl Pts',(0.430199341854858,-0.124911173756694,
0.986608710139579));
#20893=CARTESIAN_POINT('Ctrl Pts',(0.457978755888596,-0.177924977804098,
0.973971221090534));
#20894=CARTESIAN_POINT('Ctrl Pts',(0.473077587363685,-0.199697230012983,
0.966820759530997));
#20895=CARTESIAN_POINT('Ctrl Pts',(0.507057380724533,-0.237895043532788,
0.949440676105255));
#20896=CARTESIAN_POINT('Ctrl Pts',(0.525933334162555,-0.254319232363049,
0.939198248544428));
#20897=CARTESIAN_POINT('Ctrl Pts',(0.564362943424238,-0.28018331644634,
0.916597376014514));
#20898=CARTESIAN_POINT('Ctrl Pts',(0.585840553788742,-0.29104845371857,
0.903141581680914));
#20899=CARTESIAN_POINT('Ctrl Pts',(0.629305439856167,-0.30527573347708,
0.873412008702649));
#20900=CARTESIAN_POINT('Ctrl Pts',(0.651278921914856,-0.308638795020976,
0.857118508332695));
#20901=CARTESIAN_POINT('Ctrl Pts',(0.690705563850638,-0.308638795020976,
0.825676810575914));
#20902=CARTESIAN_POINT('Ctrl Pts',(0.711480111898423,-0.30527573347708,
0.807879894508811));
#20903=CARTESIAN_POINT('Ctrl Pts',(0.750136149454208,-0.29104845371857,
0.772120216227122));
#20904=CARTESIAN_POINT('Ctrl Pts',(0.768033796848072,-0.28018331644634,
0.754175290318038));
#20905=CARTESIAN_POINT('Ctrl Pts',(0.798619410861634,-0.254319232363049,
0.721738358858166));
#20906=CARTESIAN_POINT('Ctrl Pts',(0.812805334167529,-0.237895043532788,
0.705614819529209));
#20907=CARTESIAN_POINT('Ctrl Pts',(0.837310877969633,-0.199697230012983,
0.676354402927683));
#20908=CARTESIAN_POINT('Ctrl Pts',(0.847641868610495,-0.177924977804098,
0.663225258065736));
#20909=CARTESIAN_POINT('Ctrl Pts',(0.866144010579847,-0.124911173756694,
0.638954437806245));
#20910=CARTESIAN_POINT('Ctrl Pts',(0.873158080166742,-0.0925528133349865,
0.62914037979579));
#20911=CARTESIAN_POINT('Ctrl Pts',(0.876916659919095,-0.05953,0.623857181492959));
#20912=CARTESIAN_POINT('',(0.437601487681057,-0.05953,1.03511272300331));
#20913=CARTESIAN_POINT('Origin',(0.685838782044607,-0.05953,0.860014630714833));
#20914=CARTESIAN_POINT('',(0.911784794170997,-0.05953,0.656964154625313));
#20915=CARTESIAN_POINT('Ctrl Pts',(0.911784794170998,-0.0595300000000001,
0.656964154625312));
#20916=CARTESIAN_POINT('Ctrl Pts',(0.909827729890942,-0.0762225747374255,
0.659680317203144));
#20917=CARTESIAN_POINT('Ctrl Pts',(0.907004864562642,-0.0928409665394228,
0.663576540841106));
#20918=CARTESIAN_POINT('Ctrl Pts',(0.895234408667242,-0.144299303100741,
0.679480524217551));
#20919=CARTESIAN_POINT('Ctrl Pts',(0.882797231409153,-0.177024326825049,
0.695831250979106));
#20920=CARTESIAN_POINT('Ctrl Pts',(0.854332839576145,-0.227269801620064,
0.73042219438957));
#20921=CARTESIAN_POINT('Ctrl Pts',(0.834863020612702,-0.251265615809407,
0.752807465209441));
#20922=CARTESIAN_POINT('Ctrl Pts',(0.800439809856111,-0.279889827963178,
0.789147407129766));
#20923=CARTESIAN_POINT('Ctrl Pts',(0.781998747691871,-0.290879136862659,
0.80756613568454));
#20924=CARTESIAN_POINT('Ctrl Pts',(0.742239891936898,-0.305251990234487,
0.844254137480382));
#20925=CARTESIAN_POINT('Ctrl Pts',(0.720906778729541,-0.308638795020976,
0.862505527716294));
#20926=CARTESIAN_POINT('Ctrl Pts',(0.680463863683392,-0.308638795020976,
0.894757676234429));
#20927=CARTESIAN_POINT('Ctrl Pts',(0.657923009631182,-0.305251990234488,
0.91149460735272));
#20928=CARTESIAN_POINT('Ctrl Pts',(0.613307674922609,-0.290879136862659,
0.942092777160053));
#20929=CARTESIAN_POINT('Ctrl Pts',(0.591247219971725,-0.279889827963178,
0.955972930713954));
#20930=CARTESIAN_POINT('Ctrl Pts',(0.548158511259202,-0.251265615809407,
0.981446681891443));
#20931=CARTESIAN_POINT('Ctrl Pts',(0.522002043615455,-0.227269801620063,
0.995447160474328));
#20932=CARTESIAN_POINT('Ctrl Pts',(0.481944444320713,-0.177024326825049,
1.01550068154148));
#20933=CARTESIAN_POINT('Ctrl Pts',(0.463236132117164,-0.14429930310074,
1.0239876538093));
#20934=CARTESIAN_POINT('Ctrl Pts',(0.445111721969657,-0.0928409665394226,
1.03192403056628));
#20935=CARTESIAN_POINT('Ctrl Pts',(0.440685038163619,-0.0762225747374254,
1.03380912944435));
#20936=CARTESIAN_POINT('Ctrl Pts',(0.437601487681056,-0.05953,1.03511272300331));
#20937=CARTESIAN_POINT('Origin',(0.685838782044607,-0.05953,0.860014630714833));
#20938=CARTESIAN_POINT('Origin',(0.,-0.208355,0.));
#20939=CARTESIAN_POINT('',(0.0548532617164168,-0.05953,1.12247250791415));
#20940=CARTESIAN_POINT('Origin',(0.,-0.05953,0.));
#20941=CARTESIAN_POINT('',(-0.536443649899848,-0.05953,0.987512846410683));
#20942=CARTESIAN_POINT('Ctrl Pts',(0.0548532617164173,-0.0595300000000001,
1.12247250791414));
#20943=CARTESIAN_POINT('Ctrl Pts',(0.05150947068137,-0.0762225747374254,
1.12263591311425));
#20944=CARTESIAN_POINT('Ctrl Pts',(0.0467032526342597,-0.0928409665394227,
1.12285816383385));
#20945=CARTESIAN_POINT('Ctrl Pts',(0.0269302585198975,-0.144299303100741,
1.12357162229597));
#20946=CARTESIAN_POINT('Ctrl Pts',(0.006392292392153,-0.177024326825049,
1.12404235695137));
#20947=CARTESIAN_POINT('Ctrl Pts',(-0.0383992541984087,-0.227269801620063,
1.12335509974011));
#20948=CARTESIAN_POINT('Ctrl Pts',(-0.0680399972366993,-0.251265615809407,
1.12208997038458));
#20949=CARTESIAN_POINT('Ctrl Pts',(-0.117914228755037,-0.279889827963178,
1.1178344036749));
#20950=CARTESIAN_POINT('Ctrl Pts',(-0.14381238480104,-0.290879136862659,
1.11490049012186));
#20951=CARTESIAN_POINT('Ctrl Pts',(-0.19728546073067,-0.305251990234488,
1.10669035995599));
#20952=CARTESIAN_POINT('Ctrl Pts',(-0.224855950742601,-0.308638795020976,
1.10139101611326));
#20953=CARTESIAN_POINT('Ctrl Pts',(-0.275287440920027,-0.308638795020976,
1.0898803575765));
#20954=CARTESIAN_POINT('Ctrl Pts',(-0.302426893214945,-0.305251990234488,
1.08269251410343));
#20955=CARTESIAN_POINT('Ctrl Pts',(-0.35416671187353,-0.290879136862659,
1.06688848765783));
#20956=CARTESIAN_POINT('Ctrl Pts',(-0.3787731215897,-0.279889827963178,
1.05829506364875));
#20957=CARTESIAN_POINT('Ctrl Pts',(-0.425554672694338,-0.251265615809407,
1.04048957871266));
#20958=CARTESIAN_POINT('Ctrl Pts',(-0.452808978448581,-0.227269801620063,
1.02876878445619));
#20959=CARTESIAN_POINT('Ctrl Pts',(-0.493462957200432,-0.177024326825049,
1.0099536580922));
#20960=CARTESIAN_POINT('Ctrl Pts',(-0.511762781179148,-0.14429930310074,
1.00061845128527));
#20961=CARTESIAN_POINT('Ctrl Pts',(-0.529268075276157,-0.0928409665394226,
0.991396466802468));
#20962=CARTESIAN_POINT('Ctrl Pts',(-0.533501897135713,-0.0762225747374254,
0.989110885965947));
#20963=CARTESIAN_POINT('Ctrl Pts',(-0.536443649899848,-0.0595300000000001,
0.987512846410683));
#20964=CARTESIAN_POINT('',(-0.843383895613249,-0.05953,0.742736168477219));
#20965=CARTESIAN_POINT('Origin',(0.,-0.05953,0.));
#20966=CARTESIAN_POINT('',(-1.10653577764992,-0.05953,0.196295654879792));
#20967=CARTESIAN_POINT('Ctrl Pts',(-0.843383895613249,-0.0595300000000001,
0.742736168477219));
#20968=CARTESIAN_POINT('Ctrl Pts',(-0.84559647055299,-0.0762225747374255,
0.740223768851062));
#20969=CARTESIAN_POINT('Ctrl Pts',(-0.848766861100456,-0.0928409665394227,
0.736604687327351));
#20970=CARTESIAN_POINT('Ctrl Pts',(-0.861652925570091,-0.144299303100741,
0.721590372101268));
#20971=CARTESIAN_POINT('Ctrl Pts',(-0.87482617317514,-0.177024326825049,
0.705826641853758));
#20972=CARTESIAN_POINT('Ctrl Pts',(-0.902215926359523,-0.227269801620063,
0.670378702718353));
#20973=CARTESIAN_POINT('Ctrl Pts',(-0.919707509403859,-0.251265615809407,
0.646415841396062));
#20974=CARTESIAN_POINT('Ctrl Pts',(-0.947476448101718,-0.279889827963178,
0.604769294586516));
#20975=CARTESIAN_POINT('Ctrl Pts',(-0.961329858300736,-0.290879136862659,
0.582692035672022));
#20976=CARTESIAN_POINT('Ctrl Pts',(-0.988250837578047,-0.305251990234488,
0.535766169015486));
#20977=CARTESIAN_POINT('Ctrl Pts',(-1.00129756308006,-0.308638795020976,
0.510906605094603));
#20978=CARTESIAN_POINT('Ctrl Pts',(-1.02374168767024,-0.308638795020976,
0.46430090015576));
#20979=CARTESIAN_POINT('Ctrl Pts',(-1.03504317708586,-0.305251990234488,
0.438600874831839));
#20980=CARTESIAN_POINT('Ctrl Pts',(-1.05494634094458,-0.290879136862659,
0.388295406390235));
#20981=CARTESIAN_POINT('Ctrl Pts',(-1.06356957703048,-0.279889827963178,
0.363699428370917));
#20982=CARTESIAN_POINT('Ctrl Pts',(-1.0788165083757,-0.251265615809407,
0.316022600643821));
#20983=CARTESIAN_POINT('Ctrl Pts',(-1.08664560412098,-0.227269801620063,
0.287406530683752));
#20984=CARTESIAN_POINT('Ctrl Pts',(-1.09728268713976,-0.177024326825049,
0.243890930799337));
#20985=CARTESIAN_POINT('Ctrl Pts',(-1.10139388218929,-0.144299303100741,
0.22376314604679));
#20986=CARTESIAN_POINT('Ctrl Pts',(-1.10509821673782,-0.0928409665394227,
0.204327142733961));
#20987=CARTESIAN_POINT('Ctrl Pts',(-1.10595102243643,-0.0762225747374254,
0.199591971170104));
#20988=CARTESIAN_POINT('Ctrl Pts',(-1.10653577764992,-0.0595300000000001,
0.196295654879792));
#20989=CARTESIAN_POINT('',(-1.123812,-0.05953,1.37627276864339E-16));
#20990=CARTESIAN_POINT('Origin',(0.,-0.05953,0.));
#20991=CARTESIAN_POINT('',(-1.123812,-0.35718,1.37627276864339E-16));
#20992=CARTESIAN_POINT('',(-1.123812,-0.208355,1.37627276864339E-16));
#20993=CARTESIAN_POINT('Origin',(0.,-0.35718,0.));
#20994=CARTESIAN_POINT('',(-1.10653577764992,-0.05953,-0.196295654879793));
#20995=CARTESIAN_POINT('Origin',(0.,-0.05953,0.));
#20996=CARTESIAN_POINT('',(-0.843383895613249,-0.05953,-0.742736168477219));
#20997=CARTESIAN_POINT('Ctrl Pts',(-1.10653577764992,-0.0595300000000001,
-0.196295654879792));
#20998=CARTESIAN_POINT('Ctrl Pts',(-1.10595102243643,-0.0762225747374255,
-0.199591971170104));
#20999=CARTESIAN_POINT('Ctrl Pts',(-1.10509821673782,-0.0928409665394228,
-0.204327142733962));
#21000=CARTESIAN_POINT('Ctrl Pts',(-1.10139388218929,-0.144299303100741,
-0.22376314604679));
#21001=CARTESIAN_POINT('Ctrl Pts',(-1.09728268713976,-0.177024326825049,
-0.243890930799338));
#21002=CARTESIAN_POINT('Ctrl Pts',(-1.08664560412098,-0.227269801620063,
-0.287406530683753));
#21003=CARTESIAN_POINT('Ctrl Pts',(-1.0788165083757,-0.251265615809407,
-0.316022600643821));
#21004=CARTESIAN_POINT('Ctrl Pts',(-1.06356957703048,-0.279889827963178,
-0.363699428370918));
#21005=CARTESIAN_POINT('Ctrl Pts',(-1.05494634094458,-0.290879136862659,
-0.388295406390235));
#21006=CARTESIAN_POINT('Ctrl Pts',(-1.03504317708586,-0.305251990234488,
-0.438600874831839));
#21007=CARTESIAN_POINT('Ctrl Pts',(-1.02374168767024,-0.308638795020976,
-0.46430090015576));
#21008=CARTESIAN_POINT('Ctrl Pts',(-1.00129756308006,-0.308638795020976,
-0.510906605094603));
#21009=CARTESIAN_POINT('Ctrl Pts',(-0.988250837578047,-0.305251990234488,
-0.535766169015486));
#21010=CARTESIAN_POINT('Ctrl Pts',(-0.961329858300736,-0.290879136862659,
-0.582692035672022));
#21011=CARTESIAN_POINT('Ctrl Pts',(-0.947476448101718,-0.279889827963178,
-0.604769294586516));
#21012=CARTESIAN_POINT('Ctrl Pts',(-0.919707509403859,-0.251265615809407,
-0.646415841396062));
#21013=CARTESIAN_POINT('Ctrl Pts',(-0.902215926359523,-0.227269801620064,
-0.670378702718353));
#21014=CARTESIAN_POINT('Ctrl Pts',(-0.87482617317514,-0.177024326825049,
-0.705826641853758));
#21015=CARTESIAN_POINT('Ctrl Pts',(-0.861652925570091,-0.144299303100741,
-0.721590372101268));
#21016=CARTESIAN_POINT('Ctrl Pts',(-0.848766861100456,-0.0928409665394229,
-0.736604687327351));
#21017=CARTESIAN_POINT('Ctrl Pts',(-0.84559647055299,-0.0762225747374255,
-0.740223768851063));
#21018=CARTESIAN_POINT('Ctrl Pts',(-0.843383895613249,-0.0595300000000001,
-0.742736168477219));
#21019=CARTESIAN_POINT('',(-0.536443649899847,-0.05953,-0.987512846410683));
#21020=CARTESIAN_POINT('Origin',(0.,-0.05953,0.));
#21021=CARTESIAN_POINT('',(0.0548532617164172,-0.05953,-1.12247250791415));
#21022=CARTESIAN_POINT('Ctrl Pts',(-0.536443649899848,-0.0595300000000001,
-0.987512846410683));
#21023=CARTESIAN_POINT('Ctrl Pts',(-0.533501897135712,-0.0762225747374254,
-0.989110885965947));
#21024=CARTESIAN_POINT('Ctrl Pts',(-0.529268075276156,-0.0928409665394227,
-0.991396466802469));
#21025=CARTESIAN_POINT('Ctrl Pts',(-0.511762781179147,-0.144299303100741,
-1.00061845128527));
#21026=CARTESIAN_POINT('Ctrl Pts',(-0.493462957200432,-0.177024326825049,
-1.0099536580922));
#21027=CARTESIAN_POINT('Ctrl Pts',(-0.45280897844858,-0.227269801620063,
-1.02876878445619));
#21028=CARTESIAN_POINT('Ctrl Pts',(-0.425554672694337,-0.251265615809407,
-1.04048957871266));
#21029=CARTESIAN_POINT('Ctrl Pts',(-0.3787731215897,-0.279889827963178,
-1.05829506364875));
#21030=CARTESIAN_POINT('Ctrl Pts',(-0.354166711873529,-0.290879136862659,
-1.06688848765783));
#21031=CARTESIAN_POINT('Ctrl Pts',(-0.302426893214944,-0.305251990234488,
-1.08269251410343));
#21032=CARTESIAN_POINT('Ctrl Pts',(-0.275287440920027,-0.308638795020976,
-1.0898803575765));
#21033=CARTESIAN_POINT('Ctrl Pts',(-0.224855950742601,-0.308638795020976,
-1.10139101611326));
#21034=CARTESIAN_POINT('Ctrl Pts',(-0.19728546073067,-0.305251990234488,
-1.10669035995599));
#21035=CARTESIAN_POINT('Ctrl Pts',(-0.143812384801039,-0.290879136862659,
-1.11490049012186));
#21036=CARTESIAN_POINT('Ctrl Pts',(-0.117914228755037,-0.279889827963178,
-1.1178344036749));
#21037=CARTESIAN_POINT('Ctrl Pts',(-0.0680399972366989,-0.251265615809407,
-1.12208997038458));
#21038=CARTESIAN_POINT('Ctrl Pts',(-0.0383992541984084,-0.227269801620063,
-1.12335509974011));
#21039=CARTESIAN_POINT('Ctrl Pts',(0.00639229239215326,-0.177024326825049,
-1.12404235695137));
#21040=CARTESIAN_POINT('Ctrl Pts',(0.0269302585198977,-0.144299303100741,
-1.12357162229597));
#21041=CARTESIAN_POINT('Ctrl Pts',(0.04670325263426,-0.0928409665394228,
-1.12285816383385));
#21042=CARTESIAN_POINT('Ctrl Pts',(0.0515094706813703,-0.0762225747374255,
-1.12263591311425));
#21043=CARTESIAN_POINT('Ctrl Pts',(0.0548532617164176,-0.0595300000000001,
-1.12247250791414));
#21044=CARTESIAN_POINT('',(0.437601487681057,-0.05953,-1.03511272300331));
#21045=CARTESIAN_POINT('Origin',(0.,-0.05953,0.));
#21046=CARTESIAN_POINT('',(0.911784794170997,-0.05953,-0.656964154625313));
#21047=CARTESIAN_POINT('Ctrl Pts',(0.437601487681056,-0.0595300000000001,
-1.03511272300331));
#21048=CARTESIAN_POINT('Ctrl Pts',(0.440685038163619,-0.0762225747374255,
-1.03380912944435));
#21049=CARTESIAN_POINT('Ctrl Pts',(0.445111721969657,-0.0928409665394228,
-1.03192403056628));
#21050=CARTESIAN_POINT('Ctrl Pts',(0.463236132117164,-0.144299303100741,
-1.0239876538093));
#21051=CARTESIAN_POINT('Ctrl Pts',(0.481944444320713,-0.177024326825049,
-1.01550068154148));
#21052=CARTESIAN_POINT('Ctrl Pts',(0.522002043615455,-0.227269801620064,
-0.995447160474328));
#21053=CARTESIAN_POINT('Ctrl Pts',(0.548158511259203,-0.251265615809407,
-0.981446681891443));
#21054=CARTESIAN_POINT('Ctrl Pts',(0.591247219971725,-0.279889827963178,
-0.955972930713954));
#21055=CARTESIAN_POINT('Ctrl Pts',(0.613307674922609,-0.290879136862659,
-0.942092777160053));
#21056=CARTESIAN_POINT('Ctrl Pts',(0.657923009631182,-0.305251990234487,
-0.91149460735272));
#21057=CARTESIAN_POINT('Ctrl Pts',(0.680463863683393,-0.308638795020976,
-0.894757676234429));
#21058=CARTESIAN_POINT('Ctrl Pts',(0.720906778729542,-0.308638795020976,
-0.862505527716294));
#21059=CARTESIAN_POINT('Ctrl Pts',(0.742239891936899,-0.305251990234488,
-0.844254137480381));
#21060=CARTESIAN_POINT('Ctrl Pts',(0.781998747691872,-0.290879136862659,
-0.80756613568454));
#21061=CARTESIAN_POINT('Ctrl Pts',(0.800439809856112,-0.279889827963178,
-0.789147407129765));
#21062=CARTESIAN_POINT('Ctrl Pts',(0.834863020612702,-0.251265615809407,
-0.752807465209441));
#21063=CARTESIAN_POINT('Ctrl Pts',(0.854332839576145,-0.227269801620064,
-0.73042219438957));
#21064=CARTESIAN_POINT('Ctrl Pts',(0.882797231409153,-0.177024326825049,
-0.695831250979106));
#21065=CARTESIAN_POINT('Ctrl Pts',(0.895234408667242,-0.144299303100741,
-0.679480524217551));
#21066=CARTESIAN_POINT('Ctrl Pts',(0.907004864562642,-0.0928409665394228,
-0.663576540841106));
#21067=CARTESIAN_POINT('Ctrl Pts',(0.909827729890942,-0.0762225747374256,
-0.659680317203144));
#21068=CARTESIAN_POINT('Ctrl Pts',(0.911784794170998,-0.0595300000000001,
-0.656964154625312));
#21069=CARTESIAN_POINT('',(1.08212377959455,-0.05953,-0.303251606722892));
#21070=CARTESIAN_POINT('Origin',(0.,-0.05953,0.));
#21071=CARTESIAN_POINT('',(1.08212377959455,-0.05953,0.303251606722892));
#21072=CARTESIAN_POINT('Ctrl Pts',(1.08212377959455,-0.0595300000000001,
-0.303251606722892));
#21073=CARTESIAN_POINT('Ctrl Pts',(1.0830271513892,-0.0762225747374255,
-0.300028012588062));
#21074=CARTESIAN_POINT('Ctrl Pts',(1.08431331394788,-0.0928409665394228,
-0.2953917518996));
#21075=CARTESIAN_POINT('Ctrl Pts',(1.08940878963422,-0.144299303100741,
-0.276273267473431));
#21076=CARTESIAN_POINT('Ctrl Pts',(1.09443784939331,-0.177024326825049,
-0.256354979351213));
#21077=CARTESIAN_POINT('Ctrl Pts',(1.10373487993589,-0.227269801620064,
-0.212533521233765));
#21078=CARTESIAN_POINT('Ctrl Pts',(1.10909715583869,-0.251265615809407,
-0.183354415742157));
#21079=CARTESIAN_POINT('Ctrl Pts',(1.1160463456491,-0.279889827963178,-0.133783682657561));
#21080=CARTESIAN_POINT('Ctrl Pts',(1.11894887330541,-0.290879136862659,
-0.107881990270302));
#21081=CARTESIAN_POINT('Ctrl Pts',(1.12284346704144,-0.305251990234488,
-0.0539226701638766));
#21082=CARTESIAN_POINT('Ctrl Pts',(1.123812,-0.308638795020976,-0.025864214957475));
#21083=CARTESIAN_POINT('Ctrl Pts',(1.123812,-0.308638795020976,0.025864214957475));
#21084=CARTESIAN_POINT('Ctrl Pts',(1.12284346704144,-0.305251990234488,
0.0539226701638766));
#21085=CARTESIAN_POINT('Ctrl Pts',(1.11894887330541,-0.290879136862659,
0.107881990270302));
#21086=CARTESIAN_POINT('Ctrl Pts',(1.1160463456491,-0.279889827963178,0.133783682657561));
#21087=CARTESIAN_POINT('Ctrl Pts',(1.10909715583869,-0.251265615809407,
0.183354415742157));
#21088=CARTESIAN_POINT('Ctrl Pts',(1.10373487993589,-0.227269801620064,
0.212533521233765));
#21089=CARTESIAN_POINT('Ctrl Pts',(1.09443784939331,-0.177024326825049,
0.256354979351213));
#21090=CARTESIAN_POINT('Ctrl Pts',(1.08940878963422,-0.144299303100741,
0.276273267473431));
#21091=CARTESIAN_POINT('Ctrl Pts',(1.08431331394788,-0.0928409665394228,
0.2953917518996));
#21092=CARTESIAN_POINT('Ctrl Pts',(1.0830271513892,-0.0762225747374255,
0.300028012588062));
#21093=CARTESIAN_POINT('Ctrl Pts',(1.08212377959455,-0.0595300000000001,
0.303251606722892));
#21094=CARTESIAN_POINT('Origin',(0.,-0.05953,0.));
#21095=CARTESIAN_POINT('Origin',(0.,-0.05953,0.));
#21096=CARTESIAN_POINT('',(0.0589974094846122,-0.05953,1.07456964270265));
#21097=CARTESIAN_POINT('Origin',(0.,-0.05953,0.));
#21098=CARTESIAN_POINT('Origin',(-0.244773027351946,-0.05953,1.07242070340001));
#21099=CARTESIAN_POINT('Origin',(-0.244773027351946,0.,1.07242070340001));
#21100=CARTESIAN_POINT('',(-0.519393123750572,-0.05953,0.942555777842682));
#21101=CARTESIAN_POINT('Ctrl Pts',(-0.519393123750572,-0.05953,0.942555777842682));
#21102=CARTESIAN_POINT('Ctrl Pts',(-0.513714466572041,-0.0925528133349865,
0.945684988399766));
#21103=CARTESIAN_POINT('Ctrl Pts',(-0.503136848051455,-0.124911173756694,
0.951483858396181));
#21104=CARTESIAN_POINT('Ctrl Pts',(-0.47593627990192,-0.177924977804098,
0.965323333309091));
#21105=CARTESIAN_POINT('Ctrl Pts',(-0.460931856495794,-0.199697230012983,
0.972669835243841));
#21106=CARTESIAN_POINT('Ctrl Pts',(-0.426157505475872,-0.237895043532788,
0.988400002689705));
#21107=CARTESIAN_POINT('Ctrl Pts',(-0.406380688682952,-0.254319232363049,
0.996771768218699));
#21108=CARTESIAN_POINT('Ctrl Pts',(-0.364750145543744,-0.28018331644634,
1.01272583306292));
#21109=CARTESIAN_POINT('Ctrl Pts',(-0.340838910881557,-0.29104845371857,
1.02112815447116));
#21110=CARTESIAN_POINT('Ctrl Pts',(-0.290495481564827,-0.30527573347708,
1.036574285215));
#21111=CARTESIAN_POINT('Ctrl Pts',(-0.264056468041074,-0.308638795020976,
1.04359501395068));
#21112=CARTESIAN_POINT('Ctrl Pts',(-0.214892249704082,-0.308638795020976,
1.05481642595959));
#21113=CARTESIAN_POINT('Ctrl Pts',(-0.188025341585962,-0.30527573347708,
1.05996242598502));
#21114=CARTESIAN_POINT('Ctrl Pts',(-0.135965654106109,-0.29104845371857,
1.06788913840721));
#21115=CARTESIAN_POINT('Ctrl Pts',(-0.110776745452494,-0.28018331644634,
1.07069360430242));
#21116=CARTESIAN_POINT('Ctrl Pts',(-0.0663467128214646,-0.254319232363049,
1.07438230428002));
#21117=CARTESIAN_POINT('Ctrl Pts',(-0.0448960436540983,-0.237895043532788,
1.07542044338697));
#21118=CARTESIAN_POINT('Ctrl Pts',(-0.00674037211528124,-0.199697230012983,
1.07633607767727));
#21119=CARTESIAN_POINT('Ctrl Pts',(0.00996567398334777,-0.177924977804098,
1.07622728347683));
#21120=CARTESIAN_POINT('Ctrl Pts',(0.0404772621979741,-0.124911173756694,
1.07556023164702));
#21121=CARTESIAN_POINT('Ctrl Pts',(0.0525234025782719,-0.0925528133349865,
1.07492508698591));
#21122=CARTESIAN_POINT('Ctrl Pts',(0.0589974094846124,-0.05953,1.07456964270265));
#21123=CARTESIAN_POINT('Origin',(-0.244773027351946,-0.05953,1.07242070340001));
#21124=CARTESIAN_POINT('Origin',(0.,-0.05953,0.));
#21125=CARTESIAN_POINT('',(-0.803348093619616,-0.05953,0.716109245731214));
#21126=CARTESIAN_POINT('Origin',(0.,-0.05953,0.));
#21127=CARTESIAN_POINT('Origin',(-0.991065754692661,-0.05953,0.477272113029314));
#21128=CARTESIAN_POINT('Origin',(-0.991065754692661,0.,0.477272113029314));
#21129=CARTESIAN_POINT('',(-1.06075609691358,-0.05953,0.181596019242328));
#21130=CARTESIAN_POINT('Ctrl Pts',(-1.06075609691358,-0.05953,0.181596019242328));
#21131=CARTESIAN_POINT('Ctrl Pts',(-1.05966202740332,-0.0925528133349865,
0.187986803072856));
#21132=CARTESIAN_POINT('Ctrl Pts',(-1.05760072925372,-0.124911173756694,
0.199872254546857));
#21133=CARTESIAN_POINT('Ctrl Pts',(-1.05146158959546,-0.177924977804098,
0.22976728653846));
#21134=CARTESIAN_POINT('Ctrl Pts',(-1.04785021111757,-0.199697230012983,
0.246078686169301));
#21135=CARTESIAN_POINT('Ctrl Pts',(-1.03846709802406,-0.237895043532788,
0.283073967563097));
#21136=CARTESIAN_POINT('Ctrl Pts',(-1.03268176429485,-0.254319232363049,
0.303755815985685));
#21137=CARTESIAN_POINT('Ctrl Pts',(-1.01919893537026,-0.28018331644634,
0.346251081972725));
#21138=CARTESIAN_POINT('Ctrl Pts',(-1.01085972381132,-0.29104845371857,
0.370184399726282));
#21139=CARTESIAN_POINT('Ctrl Pts',(-0.99154738033959,-0.30527573347708,
0.419174982698463));
#21140=CARTESIAN_POINT('Ctrl Pts',(-0.980551951791748,-0.308638795020976,
0.444223188605045));
#21141=CARTESIAN_POINT('Ctrl Pts',(-0.958671816228589,-0.308638795020976,
0.489657758261848));
#21142=CARTESIAN_POINT('Ctrl Pts',(-0.945943877838127,-0.30527573347708,
0.51387163140139));
#21143=CARTESIAN_POINT('Ctrl Pts',(-0.91968254693063,-0.29104845371857,
0.559515758398093));
#21144=CARTESIAN_POINT('Ctrl Pts',(-0.906170138993533,-0.28018331644634,
0.580957796077825));
#21145=CARTESIAN_POINT('Ctrl Pts',(-0.8813524085237,-0.254319232363049,
0.617994461173994));
#21146=CARTESIAN_POINT('Ctrl Pts',(-0.868789784891799,-0.237895043532788,
0.635412538795143));
#21147=CARTESIAN_POINT('Ctrl Pts',(-0.845715984518854,-0.199697230012983,
0.66581473268113));
#21148=CARTESIAN_POINT('Ctrl Pts',(-0.835214876415962,-0.177924977804098,
0.678808213394124));
#21149=CARTESIAN_POINT('Ctrl Pts',(-0.815669690204649,-0.124911173756694,
0.702247233627224));
#21150=CARTESIAN_POINT('Ctrl Pts',(-0.807662468433796,-0.0925528133349865,
0.711269279199861));
#21151=CARTESIAN_POINT('Ctrl Pts',(-0.803348093619616,-0.05953,0.716109245731214));
#21152=CARTESIAN_POINT('Origin',(-0.991065754692661,-0.05953,0.477272113029314));
#21153=CARTESIAN_POINT('Origin',(0.,-0.05953,0.));
#21154=CARTESIAN_POINT('',(-1.076188,-0.05953,1.31795018948079E-16));
#21155=CARTESIAN_POINT('Origin',(0.,-0.05953,0.));
#21156=CARTESIAN_POINT('',(-1.06075609691358,-0.05953,-0.181596019242328));
#21157=CARTESIAN_POINT('Origin',(0.,-0.05953,0.));
#21158=CARTESIAN_POINT('Origin',(-0.991065754692661,-0.05953,-0.477272113029314));
#21159=CARTESIAN_POINT('Origin',(-0.991065754692661,0.,-0.477272113029314));
#21160=CARTESIAN_POINT('',(-0.803348093619616,-0.05953,-0.716109245731215));
#21161=CARTESIAN_POINT('Ctrl Pts',(-0.803348093619616,-0.05953,-0.716109245731215));
#21162=CARTESIAN_POINT('Ctrl Pts',(-0.807662468433795,-0.0925528133349865,
-0.711269279199862));
#21163=CARTESIAN_POINT('Ctrl Pts',(-0.815669690204649,-0.124911173756694,
-0.702247233627224));
#21164=CARTESIAN_POINT('Ctrl Pts',(-0.835214876415962,-0.177924977804098,
-0.678808213394124));
#21165=CARTESIAN_POINT('Ctrl Pts',(-0.845715984518854,-0.199697230012983,
-0.66581473268113));
#21166=CARTESIAN_POINT('Ctrl Pts',(-0.868789784891799,-0.237895043532788,
-0.635412538795143));
#21167=CARTESIAN_POINT('Ctrl Pts',(-0.8813524085237,-0.254319232363049,
-0.617994461173994));
#21168=CARTESIAN_POINT('Ctrl Pts',(-0.906170138993533,-0.28018331644634,
-0.580957796077826));
#21169=CARTESIAN_POINT('Ctrl Pts',(-0.91968254693063,-0.29104845371857,
-0.559515758398093));
#21170=CARTESIAN_POINT('Ctrl Pts',(-0.945943877838127,-0.30527573347708,
-0.51387163140139));
#21171=CARTESIAN_POINT('Ctrl Pts',(-0.958671816228589,-0.308638795020976,
-0.489657758261848));
#21172=CARTESIAN_POINT('Ctrl Pts',(-0.980551951791748,-0.308638795020976,
-0.444223188605045));
#21173=CARTESIAN_POINT('Ctrl Pts',(-0.99154738033959,-0.30527573347708,
-0.419174982698463));
#21174=CARTESIAN_POINT('Ctrl Pts',(-1.01085972381132,-0.29104845371857,
-0.370184399726282));
#21175=CARTESIAN_POINT('Ctrl Pts',(-1.01919893537026,-0.28018331644634,
-0.346251081972725));
#21176=CARTESIAN_POINT('Ctrl Pts',(-1.03268176429485,-0.254319232363049,
-0.303755815985685));
#21177=CARTESIAN_POINT('Ctrl Pts',(-1.03846709802406,-0.237895043532788,
-0.283073967563097));
#21178=CARTESIAN_POINT('Ctrl Pts',(-1.04785021111757,-0.199697230012983,
-0.246078686169302));
#21179=CARTESIAN_POINT('Ctrl Pts',(-1.05146158959546,-0.177924977804098,
-0.229767286538461));
#21180=CARTESIAN_POINT('Ctrl Pts',(-1.05760072925372,-0.124911173756694,
-0.199872254546858));
#21181=CARTESIAN_POINT('Ctrl Pts',(-1.05966202740332,-0.0925528133349864,
-0.187986803072857));
#21182=CARTESIAN_POINT('Ctrl Pts',(-1.06075609691358,-0.05953,-0.181596019242328));
#21183=CARTESIAN_POINT('Origin',(-0.991065754692661,-0.05953,-0.477272113029314));
#21184=CARTESIAN_POINT('Origin',(0.,-0.05953,0.));
#21185=CARTESIAN_POINT('',(-0.519393123750572,-0.05953,-0.942555777842682));
#21186=CARTESIAN_POINT('Origin',(0.,-0.05953,0.));
#21187=CARTESIAN_POINT('Origin',(-0.244773027351946,-0.05953,-1.07242070340001));
#21188=CARTESIAN_POINT('Origin',(-0.244773027351946,0.,-1.07242070340001));
#21189=CARTESIAN_POINT('',(0.0589974094846125,-0.05953,-1.07456964270265));
#21190=CARTESIAN_POINT('Ctrl Pts',(0.0589974094846127,-0.05953,-1.07456964270265));
#21191=CARTESIAN_POINT('Ctrl Pts',(0.0525234025782722,-0.0925528133349865,
-1.07492508698591));
#21192=CARTESIAN_POINT('Ctrl Pts',(0.0404772621979744,-0.124911173756694,
-1.07556023164702));
#21193=CARTESIAN_POINT('Ctrl Pts',(0.0099656739833481,-0.177924977804098,
-1.07622728347683));
#21194=CARTESIAN_POINT('Ctrl Pts',(-0.00674037211528096,-0.199697230012983,
-1.07633607767727));
#21195=CARTESIAN_POINT('Ctrl Pts',(-0.044896043654098,-0.237895043532788,
-1.07542044338697));
#21196=CARTESIAN_POINT('Ctrl Pts',(-0.0663467128214644,-0.254319232363049,
-1.07438230428002));
#21197=CARTESIAN_POINT('Ctrl Pts',(-0.110776745452493,-0.28018331644634,
-1.07069360430242));
#21198=CARTESIAN_POINT('Ctrl Pts',(-0.135965654106109,-0.29104845371857,
-1.06788913840721));
#21199=CARTESIAN_POINT('Ctrl Pts',(-0.188025341585962,-0.30527573347708,
-1.05996242598502));
#21200=CARTESIAN_POINT('Ctrl Pts',(-0.214892249704082,-0.308638795020976,
-1.05481642595959));
#21201=CARTESIAN_POINT('Ctrl Pts',(-0.264056468041074,-0.308638795020976,
-1.04359501395068));
#21202=CARTESIAN_POINT('Ctrl Pts',(-0.290495481564827,-0.30527573347708,
-1.036574285215));
#21203=CARTESIAN_POINT('Ctrl Pts',(-0.340838910881557,-0.291048453718569,
-1.02112815447116));
#21204=CARTESIAN_POINT('Ctrl Pts',(-0.364750145543744,-0.28018331644634,
-1.01272583306292));
#21205=CARTESIAN_POINT('Ctrl Pts',(-0.406380688682952,-0.254319232363049,
-0.996771768218699));
#21206=CARTESIAN_POINT('Ctrl Pts',(-0.426157505475872,-0.237895043532788,
-0.988400002689705));
#21207=CARTESIAN_POINT('Ctrl Pts',(-0.460931856495794,-0.199697230012983,
-0.972669835243841));
#21208=CARTESIAN_POINT('Ctrl Pts',(-0.475936279901919,-0.177924977804098,
-0.965323333309091));
#21209=CARTESIAN_POINT('Ctrl Pts',(-0.503136848051454,-0.124911173756694,
-0.951483858396181));
#21210=CARTESIAN_POINT('Ctrl Pts',(-0.513714466572041,-0.0925528133349865,
-0.945684988399766));
#21211=CARTESIAN_POINT('Ctrl Pts',(-0.519393123750572,-0.05953,-0.942555777842682));
#21212=CARTESIAN_POINT('Origin',(-0.244773027351946,-0.05953,-1.07242070340001));
#21213=CARTESIAN_POINT('Origin',(0.,-0.05953,0.));
#21214=CARTESIAN_POINT('',(0.413083465285518,-0.05953,-0.993751811093549));
#21215=CARTESIAN_POINT('Origin',(0.,-0.05953,0.));
#21216=CARTESIAN_POINT('Origin',(0.685838782044607,-0.05953,-0.860014630714833));
#21217=CARTESIAN_POINT('Origin',(0.685838782044607,0.,-0.860014630714833));
#21218=CARTESIAN_POINT('',(0.876916659919095,-0.05953,-0.623857181492959));
#21219=CARTESIAN_POINT('Ctrl Pts',(0.876916659919095,-0.05953,-0.623857181492958));
#21220=CARTESIAN_POINT('Ctrl Pts',(0.873158080166742,-0.0925528133349865,
-0.62914037979579));
#21221=CARTESIAN_POINT('Ctrl Pts',(0.866144010579847,-0.124911173756694,
-0.638954437806245));
#21222=CARTESIAN_POINT('Ctrl Pts',(0.847641868610495,-0.177924977804098,
-0.663225258065736));
#21223=CARTESIAN_POINT('Ctrl Pts',(0.837310877969633,-0.199697230012983,
-0.676354402927683));
#21224=CARTESIAN_POINT('Ctrl Pts',(0.81280533416753,-0.237895043532788,
-0.705614819529209));
#21225=CARTESIAN_POINT('Ctrl Pts',(0.798619410861634,-0.254319232363049,
-0.721738358858166));
#21226=CARTESIAN_POINT('Ctrl Pts',(0.768033796848072,-0.28018331644634,
-0.754175290318038));
#21227=CARTESIAN_POINT('Ctrl Pts',(0.750136149454208,-0.29104845371857,
-0.772120216227122));
#21228=CARTESIAN_POINT('Ctrl Pts',(0.711480111898423,-0.30527573347708,
-0.807879894508811));
#21229=CARTESIAN_POINT('Ctrl Pts',(0.690705563850638,-0.308638795020976,
-0.825676810575913));
#21230=CARTESIAN_POINT('Ctrl Pts',(0.651278921914856,-0.308638795020976,
-0.857118508332695));
#21231=CARTESIAN_POINT('Ctrl Pts',(0.629305439856167,-0.30527573347708,
-0.873412008702649));
#21232=CARTESIAN_POINT('Ctrl Pts',(0.585840553788742,-0.29104845371857,
-0.903141581680914));
#21233=CARTESIAN_POINT('Ctrl Pts',(0.564362943424239,-0.28018331644634,
-0.916597376014514));
#21234=CARTESIAN_POINT('Ctrl Pts',(0.525933334162556,-0.254319232363049,
-0.939198248544427));
#21235=CARTESIAN_POINT('Ctrl Pts',(0.507057380724533,-0.237895043532788,
-0.949440676105255));
#21236=CARTESIAN_POINT('Ctrl Pts',(0.473077587363686,-0.199697230012983,
-0.966820759530997));
#21237=CARTESIAN_POINT('Ctrl Pts',(0.457978755888596,-0.177924977804098,
-0.973971221090534));
#21238=CARTESIAN_POINT('Ctrl Pts',(0.430199341854858,-0.124911173756694,
-0.986608710139579));
#21239=CARTESIAN_POINT('Ctrl Pts',(0.419070565453384,-0.0925528133349865,
-0.991263089003441));
#21240=CARTESIAN_POINT('Ctrl Pts',(0.413083465285518,-0.05953,-0.993751811093549));
#21241=CARTESIAN_POINT('Origin',(0.685838782044607,-0.05953,-0.860014630714833));
#21242=CARTESIAN_POINT('Origin',(0.,-0.208355,0.));
#21243=CARTESIAN_POINT('',(-1.076188,-0.35718,1.31795018948079E-16));
#21244=CARTESIAN_POINT('Origin',(0.,-0.35718,0.));
#21245=CARTESIAN_POINT('',(-1.076188,-0.208355,1.31795018948079E-16));
#21246=CARTESIAN_POINT('',(1.03449977959455,-0.05953,0.296632461748266));
#21247=CARTESIAN_POINT('Origin',(0.,-0.05953,0.));
#21248=CARTESIAN_POINT('',(1.03449977959455,-0.05953,-0.296632461748266));
#21249=CARTESIAN_POINT('Ctrl Pts',(1.03449977959455,-0.05953,0.296632461748267));
#21250=CARTESIAN_POINT('Ctrl Pts',(1.03628691421076,-0.0925528133349865,
0.290399865505497));
#21251=CARTESIAN_POINT('Ctrl Pts',(1.03958665287714,-0.124911173756694,
0.278797079997872));
#21252=CARTESIAN_POINT('Ctrl Pts',(1.0470264474309,-0.177924977804098,0.249198913998601));
#21253=CARTESIAN_POINT('Ctrl Pts',(1.05084995891418,-0.199697230012983,
0.232935932341942));
#21254=CARTESIAN_POINT('Ctrl Pts',(1.05844771715377,-0.237895043532788,
0.195533155353269));
#21255=CARTESIAN_POINT('Ctrl Pts',(1.06220882929878,-0.254319232363049,
0.17438929156337));
#21256=CARTESIAN_POINT('Ctrl Pts',(1.06849922508772,-0.28018331644634,0.130252399648131));
#21257=CARTESIAN_POINT('Ctrl Pts',(1.07137013248666,-0.29104845371857,0.105070977154072));
#21258=CARTESIAN_POINT('Ctrl Pts',(1.07522652957392,-0.30527573347708,0.0525526752791107));
#21259=CARTESIAN_POINT('Ctrl Pts',(1.076188,-0.308638795020976,0.025214283908933));
#21260=CARTESIAN_POINT('Ctrl Pts',(1.076188,-0.308638795020976,-0.025214283908933));
#21261=CARTESIAN_POINT('Ctrl Pts',(1.07522652957392,-0.30527573347708,-0.0525526752791107));
#21262=CARTESIAN_POINT('Ctrl Pts',(1.07137013248666,-0.29104845371857,-0.105070977154072));
#21263=CARTESIAN_POINT('Ctrl Pts',(1.06849922508772,-0.28018331644634,-0.130252399648131));
#21264=CARTESIAN_POINT('Ctrl Pts',(1.06220882929878,-0.254319232363049,
-0.17438929156337));
#21265=CARTESIAN_POINT('Ctrl Pts',(1.05844771715377,-0.237895043532788,
-0.195533155353269));
#21266=CARTESIAN_POINT('Ctrl Pts',(1.05084995891418,-0.199697230012983,
-0.232935932341942));
#21267=CARTESIAN_POINT('Ctrl Pts',(1.0470264474309,-0.177924977804098,-0.249198913998601));
#21268=CARTESIAN_POINT('Ctrl Pts',(1.03958665287714,-0.124911173756694,
-0.278797079997872));
#21269=CARTESIAN_POINT('Ctrl Pts',(1.03628691421076,-0.0925528133349865,
-0.290399865505497));
#21270=CARTESIAN_POINT('Ctrl Pts',(1.03449977959455,-0.05953,-0.296632461748267));
#21271=CARTESIAN_POINT('Origin',(0.,-0.05953,0.));
#21272=CARTESIAN_POINT('Origin',(0.,-0.05953,0.));
#21273=CARTESIAN_POINT('Origin',(1.1,-0.05953,0.));
#21274=CARTESIAN_POINT('Origin',(1.1,0.,0.));
#21275=CARTESIAN_POINT('Origin',(1.1,-0.05953,0.));
#21276=CARTESIAN_POINT('Origin',(0.,-0.35718,0.));
#21277=CARTESIAN_POINT('Origin',(0.,-0.05953,0.));
#21278=CARTESIAN_POINT('',(0.,0.,0.));
#21279=CARTESIAN_POINT('Origin',(1.119765,0.495,0.));
#21280=CARTESIAN_POINT('',(-1.119765,0.495,-1.37131662304724E-16));
#21281=CARTESIAN_POINT('Origin',(0.,0.495,0.));
#21282=CARTESIAN_POINT('',(-1.085235,0.495,-1.32902956907268E-16));
#21283=CARTESIAN_POINT('Origin',(0.,0.495,0.));
#21284=CARTESIAN_POINT('Origin',(0.,0.4575,0.));
#21285=CARTESIAN_POINT('',(-1.119765,0.42,-1.37131662304724E-16));
#21286=CARTESIAN_POINT('Origin',(0.,0.42,0.));
#21287=CARTESIAN_POINT('',(-1.119765,0.4575,-1.37131662304724E-16));
#21288=CARTESIAN_POINT('Origin',(1.085235,0.42,0.));
#21289=CARTESIAN_POINT('',(-1.085235,0.42,-1.32902956907268E-16));
#21290=CARTESIAN_POINT('Origin',(0.,0.42,0.));
#21291=CARTESIAN_POINT('Origin',(0.,0.4575,0.));
#21292=CARTESIAN_POINT('',(-1.085235,0.4575,-1.32902956907268E-16));
#21293=CARTESIAN_POINT('Origin',(1.119765,-0.42,0.));
#21294=CARTESIAN_POINT('',(-1.119765,-0.42,-1.37131662304724E-16));
#21295=CARTESIAN_POINT('Origin',(0.,-0.42,0.));
#21296=CARTESIAN_POINT('',(-1.085235,-0.42,-1.32902956907268E-16));
#21297=CARTESIAN_POINT('Origin',(0.,-0.42,0.));
#21298=CARTESIAN_POINT('Origin',(0.,-0.4575,0.));
#21299=CARTESIAN_POINT('',(-1.119765,-0.495,-1.37131662304724E-16));
#21300=CARTESIAN_POINT('Origin',(0.,-0.495,0.));
#21301=CARTESIAN_POINT('',(-1.119765,-0.4575,-1.37131662304724E-16));
#21302=CARTESIAN_POINT('Origin',(1.085235,-0.495,0.));
#21303=CARTESIAN_POINT('',(-1.085235,-0.495,-1.32902956907268E-16));
#21304=CARTESIAN_POINT('Origin',(0.,-0.495,0.));
#21305=CARTESIAN_POINT('Origin',(0.,-0.4575,0.));
#21306=CARTESIAN_POINT('',(-1.085235,-0.4575,-1.32902956907268E-16));
#21307=CARTESIAN_POINT('',(0.,0.,0.));
#21308=CARTESIAN_POINT('',(0.,0.,0.));
#21309=CARTESIAN_POINT('',(0.,0.,0.));
#21310=CARTESIAN_POINT('',(0.,0.,0.));
#21311=CARTESIAN_POINT('',(0.,0.,0.));
#21312=CARTESIAN_POINT('',(0.,0.,0.));
#21313=CARTESIAN_POINT('Origin',(0.0866025403784439,-0.4,-0.15));
#21314=CARTESIAN_POINT('',(0.173205080756888,-0.4,0.));
#21315=CARTESIAN_POINT('',(0.0866025403784439,-0.4,-0.15));
#21316=CARTESIAN_POINT('',(0.173205080756888,-0.4,0.));
#21317=CARTESIAN_POINT('',(0.0866025403784439,-0.64,-0.15));
#21318=CARTESIAN_POINT('',(0.0866025403784439,-0.4,-0.15));
#21319=CARTESIAN_POINT('',(0.173205080756888,-0.64,0.));
#21320=CARTESIAN_POINT('',(0.173205080756888,-0.64,0.));
#21321=CARTESIAN_POINT('',(0.173205080756888,-0.4,0.));
#21322=CARTESIAN_POINT('Origin',(-0.0866025403784438,-0.4,-0.15));
#21323=CARTESIAN_POINT('',(-0.0866025403784438,-0.4,-0.15));
#21324=CARTESIAN_POINT('',(0.0866025403784439,-0.4,-0.15));
#21325=CARTESIAN_POINT('',(-0.0866025403784438,-0.64,-0.15));
#21326=CARTESIAN_POINT('',(-0.0866025403784438,-0.4,-0.15));
#21327=CARTESIAN_POINT('',(0.0866025403784439,-0.64,-0.15));
#21328=CARTESIAN_POINT('Origin',(-0.173205080756888,-0.4,-2.77555756156289E-17));
#21329=CARTESIAN_POINT('',(-0.173205080756888,-0.4,-2.12115047744981E-17));
#21330=CARTESIAN_POINT('',(-0.0866025403784438,-0.4,-0.15));
#21331=CARTESIAN_POINT('',(-0.173205080756888,-0.64,-2.77555756156289E-17));
#21332=CARTESIAN_POINT('',(-0.173205080756888,-0.4,-2.12115047744981E-17));
#21333=CARTESIAN_POINT('',(-0.0866025403784438,-0.64,-0.15));
#21334=CARTESIAN_POINT('Origin',(-0.0866025403784439,-0.4,0.15));
#21335=CARTESIAN_POINT('',(-0.0866025403784439,-0.4,0.15));
#21336=CARTESIAN_POINT('',(-0.173205080756888,-0.4,-2.12115047744981E-17));
#21337=CARTESIAN_POINT('',(-0.0866025403784439,-0.64,0.15));
#21338=CARTESIAN_POINT('',(-0.0866025403784439,-0.4,0.15));
#21339=CARTESIAN_POINT('',(-0.173205080756888,-0.64,-2.12115047744981E-17));
#21340=CARTESIAN_POINT('Origin',(0.0866025403784439,-0.4,0.15));
#21341=CARTESIAN_POINT('',(0.0866025403784439,-0.4,0.15));
#21342=CARTESIAN_POINT('',(-0.0866025403784439,-0.4,0.15));
#21343=CARTESIAN_POINT('',(0.0866025403784439,-0.64,0.15));
#21344=CARTESIAN_POINT('',(0.0866025403784439,-0.4,0.15));
#21345=CARTESIAN_POINT('',(-0.0866025403784439,-0.64,0.15));
#21346=CARTESIAN_POINT('Origin',(0.173205080756888,-0.4,0.));
#21347=CARTESIAN_POINT('',(0.0866025403784439,-0.4,0.15));
#21348=CARTESIAN_POINT('',(0.0866025403784439,-0.64,0.15));
#21349=CARTESIAN_POINT('Origin',(0.,-0.4,-2.77555756156289E-17));
#21350=CARTESIAN_POINT('Origin',(0.,-0.64,-2.77555756156289E-17));
#21351=CARTESIAN_POINT('Origin',(0.,-1.,0.));
#21352=CARTESIAN_POINT('',(-0.1954,-1.,2.39295984553393E-17));
#21353=CARTESIAN_POINT('Origin',(0.,-1.,0.));
#21354=CARTESIAN_POINT('Origin',(0.3,0.4,0.));
#21355=CARTESIAN_POINT('',(-0.3,0.4,-3.67394039744206E-17));
#21356=CARTESIAN_POINT('Origin',(0.,0.4,0.));
#21357=CARTESIAN_POINT('Origin',(0.,0.375,0.));
#21358=CARTESIAN_POINT('',(-0.35,0.35,-4.28626379701573E-17));
#21359=CARTESIAN_POINT('Origin',(0.,0.35,0.));
#21360=CARTESIAN_POINT('',(-0.325,0.375,-3.9801020972289E-17));
#21361=CARTESIAN_POINT('Origin',(0.,0.19,0.));
#21362=CARTESIAN_POINT('',(-0.35,0.03,-4.28626379701574E-17));
#21363=CARTESIAN_POINT('Origin',(0.,0.03,0.));
#21364=CARTESIAN_POINT('',(-0.35,0.19,-4.28626379701574E-17));
#21365=CARTESIAN_POINT('Origin',(0.,0.0149999999999999,0.));
#21366=CARTESIAN_POINT('',(-0.32,-3.29597460435593E-17,-3.91886975727153E-17));
#21367=CARTESIAN_POINT('Origin',(0.,0.,0.));
#21368=CARTESIAN_POINT('',(-0.335,0.0149999999999999,-4.10256677714363E-17));
#21369=CARTESIAN_POINT('Origin',(0.22,0.,0.));
#21370=CARTESIAN_POINT('',(-0.22,-6.93889390390723E-18,-2.69422295812418E-17));
#21371=CARTESIAN_POINT('Origin',(0.,0.,0.));
#21372=CARTESIAN_POINT('Origin',(0.,-0.02,0.));
#21373=CARTESIAN_POINT('',(-0.1954,-0.0492,2.39295984553393E-17));
#21374=CARTESIAN_POINT('Origin',(0.,-0.0492,0.));
#21375=CARTESIAN_POINT('',(-0.21,-0.02,-2.57175827820944E-17));
#21376=CARTESIAN_POINT('Origin',(0.,-0.8,0.));
#21377=CARTESIAN_POINT('',(-0.1954,-0.8,-2.39295984553393E-17));
#21378=CARTESIAN_POINT('',(0.,0.,0.));
#21379=CARTESIAN_POINT('',(0.,0.,0.));
#21380=CARTESIAN_POINT('Origin',(17.,-0.6,6.1));
#21381=CARTESIAN_POINT('',(16.775,-0.6,6.2));
#21382=CARTESIAN_POINT('Origin',(17.,-0.6,6.2));
#21383=CARTESIAN_POINT('',(16.775,-0.6,7.));
#21384=CARTESIAN_POINT('',(16.775,-0.6,6.1));
#21385=CARTESIAN_POINT('Origin',(17.,-0.6,7.));
#21386=CARTESIAN_POINT('Origin',(5.,0.6,6.1));
#21387=CARTESIAN_POINT('',(4.775,0.6,6.2));
#21388=CARTESIAN_POINT('Origin',(5.,0.6,6.2));
#21389=CARTESIAN_POINT('',(4.775,0.6,7.));
#21390=CARTESIAN_POINT('',(4.775,0.6,6.1));
#21391=CARTESIAN_POINT('Origin',(5.,0.6,7.));
#21392=CARTESIAN_POINT('Origin',(5.,-0.6,6.1));
#21393=CARTESIAN_POINT('',(4.775,-0.6,6.2));
#21394=CARTESIAN_POINT('Origin',(5.,-0.6,6.2));
#21395=CARTESIAN_POINT('',(4.775,-0.6,7.));
#21396=CARTESIAN_POINT('',(4.775,-0.6,6.1));
#21397=CARTESIAN_POINT('Origin',(5.,-0.6,7.));
#21398=CARTESIAN_POINT('Origin',(17.,0.6,6.1));
#21399=CARTESIAN_POINT('',(16.775,0.6,6.2));
#21400=CARTESIAN_POINT('Origin',(17.,0.6,6.2));
#21401=CARTESIAN_POINT('',(16.775,0.6,7.));
#21402=CARTESIAN_POINT('',(16.775,0.6,6.1));
#21403=CARTESIAN_POINT('Origin',(17.,0.6,7.));
#21404=CARTESIAN_POINT('Origin',(12.5,-1.9,6.1));
#21405=CARTESIAN_POINT('',(12.225,-1.9,6.2));
#21406=CARTESIAN_POINT('Origin',(12.5,-1.9,6.2));
#21407=CARTESIAN_POINT('',(12.225,-1.9,7.));
#21408=CARTESIAN_POINT('',(12.225,-1.9,6.1));
#21409=CARTESIAN_POINT('Origin',(12.5,-1.9,7.));
#21410=CARTESIAN_POINT('Origin',(9.5,1.9,6.1));
#21411=CARTESIAN_POINT('',(9.225,1.9,6.2));
#21412=CARTESIAN_POINT('Origin',(9.5,1.9,6.2));
#21413=CARTESIAN_POINT('',(9.225,1.9,7.));
#21414=CARTESIAN_POINT('',(9.225,1.9,6.1));
#21415=CARTESIAN_POINT('Origin',(9.5,1.9,7.));
#21416=CARTESIAN_POINT('Origin',(9.5,-1.9,6.1));
#21417=CARTESIAN_POINT('',(9.225,-1.9,6.2));
#21418=CARTESIAN_POINT('Origin',(9.5,-1.9,6.2));
#21419=CARTESIAN_POINT('',(9.225,-1.9,7.));
#21420=CARTESIAN_POINT('',(9.225,-1.9,6.1));
#21421=CARTESIAN_POINT('Origin',(9.5,-1.9,7.));
#21422=CARTESIAN_POINT('Origin',(12.5,1.9,6.1));
#21423=CARTESIAN_POINT('',(12.225,1.9,6.2));
#21424=CARTESIAN_POINT('Origin',(12.5,1.9,6.2));
#21425=CARTESIAN_POINT('',(12.225,1.9,7.));
#21426=CARTESIAN_POINT('',(12.225,1.9,6.1));
#21427=CARTESIAN_POINT('Origin',(12.5,1.9,7.));
#21428=CARTESIAN_POINT('Origin',(20.,2.5,6.2));
#21429=CARTESIAN_POINT('',(20.,2.5,6.2));
#21430=CARTESIAN_POINT('',(2.,2.5,6.2));
#21431=CARTESIAN_POINT('',(20.,2.5,6.2));
#21432=CARTESIAN_POINT('',(2.,2.5,7.));
#21433=CARTESIAN_POINT('',(2.,2.5,6.2));
#21434=CARTESIAN_POINT('',(20.,2.5,7.));
#21435=CARTESIAN_POINT('',(20.,2.5,7.));
#21436=CARTESIAN_POINT('',(20.,2.5,6.2));
#21437=CARTESIAN_POINT('Origin',(20.,-2.5,6.2));
#21438=CARTESIAN_POINT('',(20.,-2.5,6.2));
#21439=CARTESIAN_POINT('',(20.,-2.5,6.2));
#21440=CARTESIAN_POINT('',(20.,-2.5,7.));
#21441=CARTESIAN_POINT('',(20.,-2.5,7.));
#21442=CARTESIAN_POINT('',(20.,-2.5,6.2));
#21443=CARTESIAN_POINT('Origin',(2.,-2.5,6.2));
#21444=CARTESIAN_POINT('',(2.,-2.5,6.2));
#21445=CARTESIAN_POINT('',(2.,-2.5,6.2));
#21446=CARTESIAN_POINT('',(2.,-2.5,7.));
#21447=CARTESIAN_POINT('',(2.,-2.5,7.));
#21448=CARTESIAN_POINT('',(2.,-2.5,6.2));
#21449=CARTESIAN_POINT('Origin',(2.,2.5,6.2));
#21450=CARTESIAN_POINT('',(2.,2.5,6.2));
#21451=CARTESIAN_POINT('',(2.,2.5,7.));
#21452=CARTESIAN_POINT('Origin',(11.,0.,7.));
#21453=CARTESIAN_POINT('Origin',(11.,0.,6.2));
#21454=CARTESIAN_POINT('',(0.,0.,0.));
#21455=CARTESIAN_POINT('Origin',(17.,-0.6,6.9));
#21456=CARTESIAN_POINT('',(16.835,-0.6,7.));
#21457=CARTESIAN_POINT('Origin',(17.,-0.6,7.));
#21458=CARTESIAN_POINT('',(16.835,-0.6,7.9));
#21459=CARTESIAN_POINT('',(16.835,-0.6,6.9));
#21460=CARTESIAN_POINT('Origin',(17.,-0.6,7.9));
#21461=CARTESIAN_POINT('Origin',(17.,-0.6,7.9));
#21462=CARTESIAN_POINT('Origin',(5.,0.6,6.9));
#21463=CARTESIAN_POINT('',(4.835,0.6,7.));
#21464=CARTESIAN_POINT('Origin',(5.,0.6,7.));
#21465=CARTESIAN_POINT('',(4.835,0.6,7.9));
#21466=CARTESIAN_POINT('',(4.835,0.6,6.9));
#21467=CARTESIAN_POINT('Origin',(5.,0.6,7.9));
#21468=CARTESIAN_POINT('Origin',(5.,0.6,7.9));
#21469=CARTESIAN_POINT('Origin',(5.,-0.6,6.9));
#21470=CARTESIAN_POINT('',(4.835,-0.6,7.));
#21471=CARTESIAN_POINT('Origin',(5.,-0.6,7.));
#21472=CARTESIAN_POINT('',(4.835,-0.6,7.9));
#21473=CARTESIAN_POINT('',(4.835,-0.6,6.9));
#21474=CARTESIAN_POINT('Origin',(5.,-0.6,7.9));
#21475=CARTESIAN_POINT('Origin',(5.,-0.6,7.9));
#21476=CARTESIAN_POINT('Origin',(17.,0.6,6.9));
#21477=CARTESIAN_POINT('',(16.835,0.6,7.));
#21478=CARTESIAN_POINT('Origin',(17.,0.6,7.));
#21479=CARTESIAN_POINT('',(16.835,0.6,7.9));
#21480=CARTESIAN_POINT('',(16.835,0.6,6.9));
#21481=CARTESIAN_POINT('Origin',(17.,0.6,7.9));
#21482=CARTESIAN_POINT('Origin',(17.,0.6,7.9));
#21483=CARTESIAN_POINT('Origin',(1.,-1.,7.));
#21484=CARTESIAN_POINT('',(1.,-1.,8.));
#21485=CARTESIAN_POINT('',(1.,-1.,7.));
#21486=CARTESIAN_POINT('',(1.,-1.,8.));
#21487=CARTESIAN_POINT('',(1.,1.,8.));
#21488=CARTESIAN_POINT('',(1.,-1.,8.));
#21489=CARTESIAN_POINT('',(1.,1.,7.));
#21490=CARTESIAN_POINT('',(1.,1.,8.));
#21491=CARTESIAN_POINT('',(1.,-1.,7.));
#21492=CARTESIAN_POINT('Origin',(21.,-1.,7.));
#21493=CARTESIAN_POINT('',(21.,-1.,7.));
#21494=CARTESIAN_POINT('',(1.,-1.,7.));
#21495=CARTESIAN_POINT('',(21.,1.,7.));
#21496=CARTESIAN_POINT('',(1.,1.,7.));
#21497=CARTESIAN_POINT('',(21.,-1.,7.));
#21498=CARTESIAN_POINT('Origin',(21.,-1.,8.));
#21499=CARTESIAN_POINT('',(21.,-1.,8.));
#21500=CARTESIAN_POINT('',(21.,-1.,7.));
#21501=CARTESIAN_POINT('',(21.,1.,8.));
#21502=CARTESIAN_POINT('',(21.,1.,7.));
#21503=CARTESIAN_POINT('',(21.,-1.,8.));
#21504=CARTESIAN_POINT('Origin',(20.9860094173744,-1.,8.));
#21505=CARTESIAN_POINT('',(20.9860094173744,-1.,8.));
#21506=CARTESIAN_POINT('',(21.,-1.,8.));
#21507=CARTESIAN_POINT('',(20.9860094173744,1.,8.));
#21508=CARTESIAN_POINT('',(21.,1.,8.));
#21509=CARTESIAN_POINT('',(20.9860094173744,-1.,8.));
#21510=CARTESIAN_POINT('Origin',(20.8222228119546,-1.,8.45));
#21511=CARTESIAN_POINT('',(20.8222228119546,-1.,8.45));
#21512=CARTESIAN_POINT('',(20.9860094173744,-1.,8.));
#21513=CARTESIAN_POINT('',(20.8222228119546,1.,8.45));
#21514=CARTESIAN_POINT('',(20.9860094173744,1.,8.));
#21515=CARTESIAN_POINT('',(20.8222228119546,-1.,8.45));
#21516=CARTESIAN_POINT('Origin',(20.6556516403021,-1.,8.45));
#21517=CARTESIAN_POINT('',(20.6556516403021,-1.,8.45));
#21518=CARTESIAN_POINT('',(20.8222228119546,-1.,8.45));
#21519=CARTESIAN_POINT('',(20.6556516403021,1.,8.45));
#21520=CARTESIAN_POINT('',(20.8222228119546,1.,8.45));
#21521=CARTESIAN_POINT('',(20.6556516403021,-1.,8.45));
#21522=CARTESIAN_POINT('Origin',(20.4918650348823,-1.,8.));
#21523=CARTESIAN_POINT('',(20.4918650348823,-1.,8.));
#21524=CARTESIAN_POINT('',(20.6556516403021,-1.,8.45));
#21525=CARTESIAN_POINT('',(20.4918650348823,1.,8.));
#21526=CARTESIAN_POINT('',(20.6556516403021,1.,8.45));
#21527=CARTESIAN_POINT('',(20.4918650348823,-1.,8.));
#21528=CARTESIAN_POINT('Origin',(20.3576908866564,-1.,8.));
#21529=CARTESIAN_POINT('',(20.3576908866564,-1.,8.));
#21530=CARTESIAN_POINT('',(20.4918650348823,-1.,8.));
#21531=CARTESIAN_POINT('',(20.3576908866564,1.,8.));
#21532=CARTESIAN_POINT('',(20.4918650348823,1.,8.));
#21533=CARTESIAN_POINT('',(20.3576908866564,-1.,8.));
#21534=CARTESIAN_POINT('Origin',(20.1939042812366,-1.,8.45));
#21535=CARTESIAN_POINT('',(20.1939042812366,-1.,8.45));
#21536=CARTESIAN_POINT('',(20.3576908866564,-1.,8.));
#21537=CARTESIAN_POINT('',(20.1939042812366,1.,8.45));
#21538=CARTESIAN_POINT('',(20.3576908866564,1.,8.));
#21539=CARTESIAN_POINT('',(20.1939042812366,-1.,8.45));
#21540=CARTESIAN_POINT('Origin',(20.0273331095842,-1.,8.45));
#21541=CARTESIAN_POINT('',(20.0273331095842,-1.,8.45));
#21542=CARTESIAN_POINT('',(20.1939042812366,-1.,8.45));
#21543=CARTESIAN_POINT('',(20.0273331095842,1.,8.45));
#21544=CARTESIAN_POINT('',(20.1939042812366,1.,8.45));
#21545=CARTESIAN_POINT('',(20.0273331095842,-1.,8.45));
#21546=CARTESIAN_POINT('Origin',(19.8635465041644,-1.,8.));
#21547=CARTESIAN_POINT('',(19.8635465041644,-1.,8.));
#21548=CARTESIAN_POINT('',(20.0273331095842,-1.,8.45));
#21549=CARTESIAN_POINT('',(19.8635465041644,1.,8.));
#21550=CARTESIAN_POINT('',(20.0273331095842,1.,8.45));
#21551=CARTESIAN_POINT('',(19.8635465041644,-1.,8.));
#21552=CARTESIAN_POINT('Origin',(19.7293723559385,-1.,8.));
#21553=CARTESIAN_POINT('',(19.7293723559385,-1.,8.));
#21554=CARTESIAN_POINT('',(19.8635465041644,-1.,8.));
#21555=CARTESIAN_POINT('',(19.7293723559385,1.,8.));
#21556=CARTESIAN_POINT('',(19.8635465041644,1.,8.));
#21557=CARTESIAN_POINT('',(19.7293723559385,-1.,8.));
#21558=CARTESIAN_POINT('Origin',(19.5655857505187,-1.,8.45));
#21559=CARTESIAN_POINT('',(19.5655857505187,-1.,8.45));
#21560=CARTESIAN_POINT('',(19.7293723559385,-1.,8.));
#21561=CARTESIAN_POINT('',(19.5655857505187,1.,8.45));
#21562=CARTESIAN_POINT('',(19.7293723559385,1.,8.));
#21563=CARTESIAN_POINT('',(19.5655857505187,-1.,8.45));
#21564=CARTESIAN_POINT('Origin',(19.3990145788662,-1.,8.45));
#21565=CARTESIAN_POINT('',(19.3990145788662,-1.,8.45));
#21566=CARTESIAN_POINT('',(19.5655857505187,-1.,8.45));
#21567=CARTESIAN_POINT('',(19.3990145788662,1.,8.45));
#21568=CARTESIAN_POINT('',(19.5655857505187,1.,8.45));
#21569=CARTESIAN_POINT('',(19.3990145788662,-1.,8.45));
#21570=CARTESIAN_POINT('Origin',(19.2352279734464,-1.,8.));
#21571=CARTESIAN_POINT('',(19.2352279734464,-1.,8.));
#21572=CARTESIAN_POINT('',(19.3990145788662,-1.,8.45));
#21573=CARTESIAN_POINT('',(19.2352279734464,1.,8.));
#21574=CARTESIAN_POINT('',(19.3990145788662,1.,8.45));
#21575=CARTESIAN_POINT('',(19.2352279734464,-1.,8.));
#21576=CARTESIAN_POINT('Origin',(19.1010538252205,-1.,8.));
#21577=CARTESIAN_POINT('',(19.1010538252205,-1.,8.));
#21578=CARTESIAN_POINT('',(19.2352279734464,-1.,8.));
#21579=CARTESIAN_POINT('',(19.1010538252205,1.,8.));
#21580=CARTESIAN_POINT('',(19.2352279734464,1.,8.));
#21581=CARTESIAN_POINT('',(19.1010538252205,-1.,8.));
#21582=CARTESIAN_POINT('Origin',(18.9372672198007,-1.,8.45));
#21583=CARTESIAN_POINT('',(18.9372672198007,-1.,8.45));
#21584=CARTESIAN_POINT('',(19.1010538252205,-1.,8.));
#21585=CARTESIAN_POINT('',(18.9372672198007,1.,8.45));
#21586=CARTESIAN_POINT('',(19.1010538252205,1.,8.));
#21587=CARTESIAN_POINT('',(18.9372672198007,-1.,8.45));
#21588=CARTESIAN_POINT('Origin',(18.7706960481482,-1.,8.45));
#21589=CARTESIAN_POINT('',(18.7706960481482,-1.,8.45));
#21590=CARTESIAN_POINT('',(18.9372672198007,-1.,8.45));
#21591=CARTESIAN_POINT('',(18.7706960481482,1.,8.45));
#21592=CARTESIAN_POINT('',(18.9372672198007,1.,8.45));
#21593=CARTESIAN_POINT('',(18.7706960481482,-1.,8.45));
#21594=CARTESIAN_POINT('Origin',(18.6069094427284,-1.,8.));
#21595=CARTESIAN_POINT('',(18.6069094427284,-1.,8.));
#21596=CARTESIAN_POINT('',(18.7706960481482,-1.,8.45));
#21597=CARTESIAN_POINT('',(18.6069094427284,1.,8.));
#21598=CARTESIAN_POINT('',(18.7706960481482,1.,8.45));
#21599=CARTESIAN_POINT('',(18.6069094427284,-1.,8.));
#21600=CARTESIAN_POINT('Origin',(18.4727352945026,-1.,8.));
#21601=CARTESIAN_POINT('',(18.4727352945026,-1.,8.));
#21602=CARTESIAN_POINT('',(18.6069094427284,-1.,8.));
#21603=CARTESIAN_POINT('',(18.4727352945026,1.,8.));
#21604=CARTESIAN_POINT('',(18.6069094427284,1.,8.));
#21605=CARTESIAN_POINT('',(18.4727352945026,-1.,8.));
#21606=CARTESIAN_POINT('Origin',(18.3089486890828,-1.,8.45));
#21607=CARTESIAN_POINT('',(18.3089486890828,-1.,8.45));
#21608=CARTESIAN_POINT('',(18.4727352945026,-1.,8.));
#21609=CARTESIAN_POINT('',(18.3089486890828,1.,8.45));
#21610=CARTESIAN_POINT('',(18.4727352945026,1.,8.));
#21611=CARTESIAN_POINT('',(18.3089486890828,-1.,8.45));
#21612=CARTESIAN_POINT('Origin',(18.1423775174303,-1.,8.45));
#21613=CARTESIAN_POINT('',(18.1423775174303,-1.,8.45));
#21614=CARTESIAN_POINT('',(18.3089486890828,-1.,8.45));
#21615=CARTESIAN_POINT('',(18.1423775174303,1.,8.45));
#21616=CARTESIAN_POINT('',(18.3089486890828,1.,8.45));
#21617=CARTESIAN_POINT('',(18.1423775174303,-1.,8.45));
#21618=CARTESIAN_POINT('Origin',(17.9785909120105,-1.,8.));
#21619=CARTESIAN_POINT('',(17.9785909120105,-1.,8.));
#21620=CARTESIAN_POINT('',(18.1423775174303,-1.,8.45));
#21621=CARTESIAN_POINT('',(17.9785909120105,1.,8.));
#21622=CARTESIAN_POINT('',(18.1423775174303,1.,8.45));
#21623=CARTESIAN_POINT('',(17.9785909120105,-1.,8.));
#21624=CARTESIAN_POINT('Origin',(17.8444167637846,-1.,8.));
#21625=CARTESIAN_POINT('',(17.8444167637846,-1.,8.));
#21626=CARTESIAN_POINT('',(17.9785909120105,-1.,8.));
#21627=CARTESIAN_POINT('',(17.8444167637846,1.,8.));
#21628=CARTESIAN_POINT('',(17.9785909120105,1.,8.));
#21629=CARTESIAN_POINT('',(17.8444167637846,-1.,8.));
#21630=CARTESIAN_POINT('Origin',(17.6806301583648,-1.,8.45));
#21631=CARTESIAN_POINT('',(17.6806301583648,-1.,8.45));
#21632=CARTESIAN_POINT('',(17.8444167637846,-1.,8.));
#21633=CARTESIAN_POINT('',(17.6806301583648,1.,8.45));
#21634=CARTESIAN_POINT('',(17.8444167637846,1.,8.));
#21635=CARTESIAN_POINT('',(17.6806301583648,-1.,8.45));
#21636=CARTESIAN_POINT('Origin',(17.5140589867123,-1.,8.45));
#21637=CARTESIAN_POINT('',(17.5140589867123,-1.,8.45));
#21638=CARTESIAN_POINT('',(17.6806301583648,-1.,8.45));
#21639=CARTESIAN_POINT('',(17.5140589867123,1.,8.45));
#21640=CARTESIAN_POINT('',(17.6806301583648,1.,8.45));
#21641=CARTESIAN_POINT('',(17.5140589867123,-1.,8.45));
#21642=CARTESIAN_POINT('Origin',(17.3502723812925,-1.,8.));
#21643=CARTESIAN_POINT('',(17.3502723812925,-1.,8.));
#21644=CARTESIAN_POINT('',(17.5140589867123,-1.,8.45));
#21645=CARTESIAN_POINT('',(17.3502723812925,1.,8.));
#21646=CARTESIAN_POINT('',(17.5140589867123,1.,8.45));
#21647=CARTESIAN_POINT('',(17.3502723812925,-1.,8.));
#21648=CARTESIAN_POINT('Origin',(17.2160982330666,-1.,8.));
#21649=CARTESIAN_POINT('',(17.2160982330666,-1.,8.));
#21650=CARTESIAN_POINT('',(17.3502723812925,-1.,8.));
#21651=CARTESIAN_POINT('',(17.2160982330666,1.,8.));
#21652=CARTESIAN_POINT('',(17.3502723812925,1.,8.));
#21653=CARTESIAN_POINT('',(17.2160982330666,-1.,8.));
#21654=CARTESIAN_POINT('Origin',(17.0523116276469,-1.,8.45));
#21655=CARTESIAN_POINT('',(17.0523116276469,-1.,8.45));
#21656=CARTESIAN_POINT('',(17.2160982330666,-1.,8.));
#21657=CARTESIAN_POINT('',(17.0523116276469,1.,8.45));
#21658=CARTESIAN_POINT('',(17.2160982330666,1.,8.));
#21659=CARTESIAN_POINT('',(17.0523116276469,-1.,8.45));
#21660=CARTESIAN_POINT('Origin',(16.8857404559944,-1.,8.45));
#21661=CARTESIAN_POINT('',(16.8857404559944,-1.,8.45));
#21662=CARTESIAN_POINT('',(17.0523116276469,-1.,8.45));
#21663=CARTESIAN_POINT('',(16.8857404559944,1.,8.45));
#21664=CARTESIAN_POINT('',(17.0523116276469,1.,8.45));
#21665=CARTESIAN_POINT('',(16.8857404559944,-1.,8.45));
#21666=CARTESIAN_POINT('Origin',(16.7219538505746,-1.,8.));
#21667=CARTESIAN_POINT('',(16.7219538505746,-1.,8.));
#21668=CARTESIAN_POINT('',(16.8857404559944,-1.,8.45));
#21669=CARTESIAN_POINT('',(16.7219538505746,1.,8.));
#21670=CARTESIAN_POINT('',(16.8857404559944,1.,8.45));
#21671=CARTESIAN_POINT('',(16.7219538505746,-1.,8.));
#21672=CARTESIAN_POINT('Origin',(16.5877797023487,-1.,8.));
#21673=CARTESIAN_POINT('',(16.5877797023487,-1.,8.));
#21674=CARTESIAN_POINT('',(16.7219538505746,-1.,8.));
#21675=CARTESIAN_POINT('',(16.5877797023487,1.,8.));
#21676=CARTESIAN_POINT('',(16.7219538505746,1.,8.));
#21677=CARTESIAN_POINT('',(16.5877797023487,-1.,8.));
#21678=CARTESIAN_POINT('Origin',(16.4239930969289,-1.,8.45));
#21679=CARTESIAN_POINT('',(16.4239930969289,-1.,8.45));
#21680=CARTESIAN_POINT('',(16.5877797023487,-1.,8.));
#21681=CARTESIAN_POINT('',(16.4239930969289,1.,8.45));
#21682=CARTESIAN_POINT('',(16.5877797023487,1.,8.));
#21683=CARTESIAN_POINT('',(16.4239930969289,-1.,8.45));
#21684=CARTESIAN_POINT('Origin',(16.2574219252764,-1.,8.45));
#21685=CARTESIAN_POINT('',(16.2574219252764,-1.,8.45));
#21686=CARTESIAN_POINT('',(16.4239930969289,-1.,8.45));
#21687=CARTESIAN_POINT('',(16.2574219252764,1.,8.45));
#21688=CARTESIAN_POINT('',(16.4239930969289,1.,8.45));
#21689=CARTESIAN_POINT('',(16.2574219252764,-1.,8.45));
#21690=CARTESIAN_POINT('Origin',(16.0936353198566,-1.,8.));
#21691=CARTESIAN_POINT('',(16.0936353198566,-1.,8.));
#21692=CARTESIAN_POINT('',(16.2574219252764,-1.,8.45));
#21693=CARTESIAN_POINT('',(16.0936353198566,1.,8.));
#21694=CARTESIAN_POINT('',(16.2574219252764,1.,8.45));
#21695=CARTESIAN_POINT('',(16.0936353198566,-1.,8.));
#21696=CARTESIAN_POINT('Origin',(15.9594611716307,-1.,8.));
#21697=CARTESIAN_POINT('',(15.9594611716307,-1.,8.));
#21698=CARTESIAN_POINT('',(16.0936353198566,-1.,8.));
#21699=CARTESIAN_POINT('',(15.9594611716307,1.,8.));
#21700=CARTESIAN_POINT('',(16.0936353198566,1.,8.));
#21701=CARTESIAN_POINT('',(15.9594611716307,-1.,8.));
#21702=CARTESIAN_POINT('Origin',(15.7956745662109,-1.,8.45));
#21703=CARTESIAN_POINT('',(15.7956745662109,-1.,8.45));
#21704=CARTESIAN_POINT('',(15.9594611716307,-1.,8.));
#21705=CARTESIAN_POINT('',(15.7956745662109,1.,8.45));
#21706=CARTESIAN_POINT('',(15.9594611716307,1.,8.));
#21707=CARTESIAN_POINT('',(15.7956745662109,-1.,8.45));
#21708=CARTESIAN_POINT('Origin',(15.6291033945584,-1.,8.45));
#21709=CARTESIAN_POINT('',(15.6291033945584,-1.,8.45));
#21710=CARTESIAN_POINT('',(15.7956745662109,-1.,8.45));
#21711=CARTESIAN_POINT('',(15.6291033945584,1.,8.45));
#21712=CARTESIAN_POINT('',(15.7956745662109,1.,8.45));
#21713=CARTESIAN_POINT('',(15.6291033945584,-1.,8.45));
#21714=CARTESIAN_POINT('Origin',(15.4653167891387,-1.,8.));
#21715=CARTESIAN_POINT('',(15.4653167891387,-1.,8.));
#21716=CARTESIAN_POINT('',(15.6291033945584,-1.,8.45));
#21717=CARTESIAN_POINT('',(15.4653167891387,1.,8.));
#21718=CARTESIAN_POINT('',(15.6291033945584,1.,8.45));
#21719=CARTESIAN_POINT('',(15.4653167891387,-1.,8.));
#21720=CARTESIAN_POINT('Origin',(15.3311426409128,-1.,8.));
#21721=CARTESIAN_POINT('',(15.3311426409128,-1.,8.));
#21722=CARTESIAN_POINT('',(15.4653167891387,-1.,8.));
#21723=CARTESIAN_POINT('',(15.3311426409128,1.,8.));
#21724=CARTESIAN_POINT('',(15.4653167891387,1.,8.));
#21725=CARTESIAN_POINT('',(15.3311426409128,-1.,8.));
#21726=CARTESIAN_POINT('Origin',(15.167356035493,-1.,8.45));
#21727=CARTESIAN_POINT('',(15.167356035493,-1.,8.45));
#21728=CARTESIAN_POINT('',(15.3311426409128,-1.,8.));
#21729=CARTESIAN_POINT('',(15.167356035493,1.,8.45));
#21730=CARTESIAN_POINT('',(15.3311426409128,1.,8.));
#21731=CARTESIAN_POINT('',(15.167356035493,-1.,8.45));
#21732=CARTESIAN_POINT('Origin',(15.0007848638405,-1.,8.45));
#21733=CARTESIAN_POINT('',(15.0007848638405,-1.,8.45));
#21734=CARTESIAN_POINT('',(15.167356035493,-1.,8.45));
#21735=CARTESIAN_POINT('',(15.0007848638405,1.,8.45));
#21736=CARTESIAN_POINT('',(15.167356035493,1.,8.45));
#21737=CARTESIAN_POINT('',(15.0007848638405,-1.,8.45));
#21738=CARTESIAN_POINT('Origin',(14.8369982584207,-1.,8.));
#21739=CARTESIAN_POINT('',(14.8369982584207,-1.,8.));
#21740=CARTESIAN_POINT('',(15.0007848638405,-1.,8.45));
#21741=CARTESIAN_POINT('',(14.8369982584207,1.,8.));
#21742=CARTESIAN_POINT('',(15.0007848638405,1.,8.45));
#21743=CARTESIAN_POINT('',(14.8369982584207,-1.,8.));
#21744=CARTESIAN_POINT('Origin',(14.7028241101948,-1.,8.));
#21745=CARTESIAN_POINT('',(14.7028241101948,-1.,8.));
#21746=CARTESIAN_POINT('',(14.8369982584207,-1.,8.));
#21747=CARTESIAN_POINT('',(14.7028241101948,1.,8.));
#21748=CARTESIAN_POINT('',(14.8369982584207,1.,8.));
#21749=CARTESIAN_POINT('',(14.7028241101948,-1.,8.));
#21750=CARTESIAN_POINT('Origin',(14.539037504775,-1.,8.45));
#21751=CARTESIAN_POINT('',(14.539037504775,-1.,8.45));
#21752=CARTESIAN_POINT('',(14.7028241101948,-1.,8.));
#21753=CARTESIAN_POINT('',(14.539037504775,1.,8.45));
#21754=CARTESIAN_POINT('',(14.7028241101948,1.,8.));
#21755=CARTESIAN_POINT('',(14.539037504775,-1.,8.45));
#21756=CARTESIAN_POINT('Origin',(14.3724663331225,-1.,8.45));
#21757=CARTESIAN_POINT('',(14.3724663331225,-1.,8.45));
#21758=CARTESIAN_POINT('',(14.539037504775,-1.,8.45));
#21759=CARTESIAN_POINT('',(14.3724663331225,1.,8.45));
#21760=CARTESIAN_POINT('',(14.539037504775,1.,8.45));
#21761=CARTESIAN_POINT('',(14.3724663331225,-1.,8.45));
#21762=CARTESIAN_POINT('Origin',(14.2086797277027,-1.,8.));
#21763=CARTESIAN_POINT('',(14.2086797277027,-1.,8.));
#21764=CARTESIAN_POINT('',(14.3724663331225,-1.,8.45));
#21765=CARTESIAN_POINT('',(14.2086797277027,1.,8.));
#21766=CARTESIAN_POINT('',(14.3724663331225,1.,8.45));
#21767=CARTESIAN_POINT('',(14.2086797277027,-1.,8.));
#21768=CARTESIAN_POINT('Origin',(14.0745055794769,-1.,8.));
#21769=CARTESIAN_POINT('',(14.0745055794769,-1.,8.));
#21770=CARTESIAN_POINT('',(14.2086797277027,-1.,8.));
#21771=CARTESIAN_POINT('',(14.0745055794769,1.,8.));
#21772=CARTESIAN_POINT('',(14.2086797277027,1.,8.));
#21773=CARTESIAN_POINT('',(14.0745055794769,-1.,8.));
#21774=CARTESIAN_POINT('Origin',(13.9107189740571,-1.,8.45));
#21775=CARTESIAN_POINT('',(13.9107189740571,-1.,8.45));
#21776=CARTESIAN_POINT('',(14.0745055794769,-1.,8.));
#21777=CARTESIAN_POINT('',(13.9107189740571,1.,8.45));
#21778=CARTESIAN_POINT('',(14.0745055794769,1.,8.));
#21779=CARTESIAN_POINT('',(13.9107189740571,-1.,8.45));
#21780=CARTESIAN_POINT('Origin',(13.7441478024046,-1.,8.45));
#21781=CARTESIAN_POINT('',(13.7441478024046,-1.,8.45));
#21782=CARTESIAN_POINT('',(13.9107189740571,-1.,8.45));
#21783=CARTESIAN_POINT('',(13.7441478024046,1.,8.45));
#21784=CARTESIAN_POINT('',(13.9107189740571,1.,8.45));
#21785=CARTESIAN_POINT('',(13.7441478024046,-1.,8.45));
#21786=CARTESIAN_POINT('Origin',(13.5803611969848,-1.,8.));
#21787=CARTESIAN_POINT('',(13.5803611969848,-1.,8.));
#21788=CARTESIAN_POINT('',(13.7441478024046,-1.,8.45));
#21789=CARTESIAN_POINT('',(13.5803611969848,1.,8.));
#21790=CARTESIAN_POINT('',(13.7441478024046,1.,8.45));
#21791=CARTESIAN_POINT('',(13.5803611969848,-1.,8.));
#21792=CARTESIAN_POINT('Origin',(13.4461870487589,-1.,8.));
#21793=CARTESIAN_POINT('',(13.4461870487589,-1.,8.));
#21794=CARTESIAN_POINT('',(13.5803611969848,-1.,8.));
#21795=CARTESIAN_POINT('',(13.4461870487589,1.,8.));
#21796=CARTESIAN_POINT('',(13.5803611969848,1.,8.));
#21797=CARTESIAN_POINT('',(13.4461870487589,-1.,8.));
#21798=CARTESIAN_POINT('Origin',(13.2824004433391,-1.,8.45));
#21799=CARTESIAN_POINT('',(13.2824004433391,-1.,8.45));
#21800=CARTESIAN_POINT('',(13.4461870487589,-1.,8.));
#21801=CARTESIAN_POINT('',(13.2824004433391,1.,8.45));
#21802=CARTESIAN_POINT('',(13.4461870487589,1.,8.));
#21803=CARTESIAN_POINT('',(13.2824004433391,-1.,8.45));
#21804=CARTESIAN_POINT('Origin',(13.1158292716866,-1.,8.45));
#21805=CARTESIAN_POINT('',(13.1158292716866,-1.,8.45));
#21806=CARTESIAN_POINT('',(13.2824004433391,-1.,8.45));
#21807=CARTESIAN_POINT('',(13.1158292716866,1.,8.45));
#21808=CARTESIAN_POINT('',(13.2824004433391,1.,8.45));
#21809=CARTESIAN_POINT('',(13.1158292716866,-1.,8.45));
#21810=CARTESIAN_POINT('Origin',(12.9520426662668,-1.,8.));
#21811=CARTESIAN_POINT('',(12.9520426662668,-1.,8.));
#21812=CARTESIAN_POINT('',(13.1158292716866,-1.,8.45));
#21813=CARTESIAN_POINT('',(12.9520426662668,1.,8.));
#21814=CARTESIAN_POINT('',(13.1158292716866,1.,8.45));
#21815=CARTESIAN_POINT('',(12.9520426662668,-1.,8.));
#21816=CARTESIAN_POINT('Origin',(12.8178685180409,-1.,8.));
#21817=CARTESIAN_POINT('',(12.8178685180409,-1.,8.));
#21818=CARTESIAN_POINT('',(12.9520426662668,-1.,8.));
#21819=CARTESIAN_POINT('',(12.8178685180409,1.,8.));
#21820=CARTESIAN_POINT('',(12.9520426662668,1.,8.));
#21821=CARTESIAN_POINT('',(12.8178685180409,-1.,8.));
#21822=CARTESIAN_POINT('Origin',(12.6540819126211,-1.,8.45));
#21823=CARTESIAN_POINT('',(12.6540819126211,-1.,8.45));
#21824=CARTESIAN_POINT('',(12.8178685180409,-1.,8.));
#21825=CARTESIAN_POINT('',(12.6540819126211,1.,8.45));
#21826=CARTESIAN_POINT('',(12.8178685180409,1.,8.));
#21827=CARTESIAN_POINT('',(12.6540819126211,-1.,8.45));
#21828=CARTESIAN_POINT('Origin',(12.4875107409686,-1.,8.45));
#21829=CARTESIAN_POINT('',(12.4875107409686,-1.,8.45));
#21830=CARTESIAN_POINT('',(12.6540819126211,-1.,8.45));
#21831=CARTESIAN_POINT('',(12.4875107409686,1.,8.45));
#21832=CARTESIAN_POINT('',(12.6540819126211,1.,8.45));
#21833=CARTESIAN_POINT('',(12.4875107409686,-1.,8.45));
#21834=CARTESIAN_POINT('Origin',(12.3237241355489,-1.,8.));
#21835=CARTESIAN_POINT('',(12.3237241355489,-1.,8.));
#21836=CARTESIAN_POINT('',(12.4875107409686,-1.,8.45));
#21837=CARTESIAN_POINT('',(12.3237241355489,1.,8.));
#21838=CARTESIAN_POINT('',(12.4875107409686,1.,8.45));
#21839=CARTESIAN_POINT('',(12.3237241355489,-1.,8.));
#21840=CARTESIAN_POINT('Origin',(12.189549987323,-1.,8.));
#21841=CARTESIAN_POINT('',(12.189549987323,-1.,8.));
#21842=CARTESIAN_POINT('',(12.3237241355489,-1.,8.));
#21843=CARTESIAN_POINT('',(12.189549987323,1.,8.));
#21844=CARTESIAN_POINT('',(12.3237241355489,1.,8.));
#21845=CARTESIAN_POINT('',(12.189549987323,-1.,8.));
#21846=CARTESIAN_POINT('Origin',(12.0257633819032,-1.,8.45));
#21847=CARTESIAN_POINT('',(12.0257633819032,-1.,8.45));
#21848=CARTESIAN_POINT('',(12.189549987323,-1.,8.));
#21849=CARTESIAN_POINT('',(12.0257633819032,1.,8.45));
#21850=CARTESIAN_POINT('',(12.189549987323,1.,8.));
#21851=CARTESIAN_POINT('',(12.0257633819032,-1.,8.45));
#21852=CARTESIAN_POINT('Origin',(11.8591922102507,-1.,8.45));
#21853=CARTESIAN_POINT('',(11.8591922102507,-1.,8.45));
#21854=CARTESIAN_POINT('',(12.0257633819032,-1.,8.45));
#21855=CARTESIAN_POINT('',(11.8591922102507,1.,8.45));
#21856=CARTESIAN_POINT('',(12.0257633819032,1.,8.45));
#21857=CARTESIAN_POINT('',(11.8591922102507,-1.,8.45));
#21858=CARTESIAN_POINT('Origin',(11.6954056048309,-1.,8.));
#21859=CARTESIAN_POINT('',(11.6954056048309,-1.,8.));
#21860=CARTESIAN_POINT('',(11.8591922102507,-1.,8.45));
#21861=CARTESIAN_POINT('',(11.6954056048309,1.,8.));
#21862=CARTESIAN_POINT('',(11.8591922102507,1.,8.45));
#21863=CARTESIAN_POINT('',(11.6954056048309,-1.,8.));
#21864=CARTESIAN_POINT('Origin',(11.561231456605,-1.,8.));
#21865=CARTESIAN_POINT('',(11.561231456605,-1.,8.));
#21866=CARTESIAN_POINT('',(11.6954056048309,-1.,8.));
#21867=CARTESIAN_POINT('',(11.561231456605,1.,8.));
#21868=CARTESIAN_POINT('',(11.6954056048309,1.,8.));
#21869=CARTESIAN_POINT('',(11.561231456605,-1.,8.));
#21870=CARTESIAN_POINT('Origin',(11.3974448511852,-1.,8.45));
#21871=CARTESIAN_POINT('',(11.3974448511852,-1.,8.45));
#21872=CARTESIAN_POINT('',(11.561231456605,-1.,8.));
#21873=CARTESIAN_POINT('',(11.3974448511852,1.,8.45));
#21874=CARTESIAN_POINT('',(11.561231456605,1.,8.));
#21875=CARTESIAN_POINT('',(11.3974448511852,-1.,8.45));
#21876=CARTESIAN_POINT('Origin',(11.2308736795327,-1.,8.45));
#21877=CARTESIAN_POINT('',(11.2308736795327,-1.,8.45));
#21878=CARTESIAN_POINT('',(11.3974448511852,-1.,8.45));
#21879=CARTESIAN_POINT('',(11.2308736795327,1.,8.45));
#21880=CARTESIAN_POINT('',(11.3974448511852,1.,8.45));
#21881=CARTESIAN_POINT('',(11.2308736795327,-1.,8.45));
#21882=CARTESIAN_POINT('Origin',(11.0670870741129,-1.,8.));
#21883=CARTESIAN_POINT('',(11.0670870741129,-1.,8.));
#21884=CARTESIAN_POINT('',(11.2308736795327,-1.,8.45));
#21885=CARTESIAN_POINT('',(11.0670870741129,1.,8.));
#21886=CARTESIAN_POINT('',(11.2308736795327,1.,8.45));
#21887=CARTESIAN_POINT('',(11.0670870741129,-1.,8.));
#21888=CARTESIAN_POINT('Origin',(10.9329129258871,-1.,8.));
#21889=CARTESIAN_POINT('',(10.9329129258871,-1.,8.));
#21890=CARTESIAN_POINT('',(11.0670870741129,-1.,8.));
#21891=CARTESIAN_POINT('',(10.9329129258871,1.,8.));
#21892=CARTESIAN_POINT('',(11.0670870741129,1.,8.));
#21893=CARTESIAN_POINT('',(10.9329129258871,-1.,8.));
#21894=CARTESIAN_POINT('Origin',(10.7691263204673,-1.,8.45));
#21895=CARTESIAN_POINT('',(10.7691263204673,-1.,8.45));
#21896=CARTESIAN_POINT('',(10.9329129258871,-1.,8.));
#21897=CARTESIAN_POINT('',(10.7691263204673,1.,8.45));
#21898=CARTESIAN_POINT('',(10.9329129258871,1.,8.));
#21899=CARTESIAN_POINT('',(10.7691263204673,-1.,8.45));
#21900=CARTESIAN_POINT('Origin',(10.6025551488148,-1.,8.45));
#21901=CARTESIAN_POINT('',(10.6025551488148,-1.,8.45));
#21902=CARTESIAN_POINT('',(10.7691263204673,-1.,8.45));
#21903=CARTESIAN_POINT('',(10.6025551488148,1.,8.45));
#21904=CARTESIAN_POINT('',(10.7691263204673,1.,8.45));
#21905=CARTESIAN_POINT('',(10.6025551488148,-1.,8.45));
#21906=CARTESIAN_POINT('Origin',(10.438768543395,-1.,8.));
#21907=CARTESIAN_POINT('',(10.438768543395,-1.,8.));
#21908=CARTESIAN_POINT('',(10.6025551488148,-1.,8.45));
#21909=CARTESIAN_POINT('',(10.438768543395,1.,8.));
#21910=CARTESIAN_POINT('',(10.6025551488148,1.,8.45));
#21911=CARTESIAN_POINT('',(10.438768543395,-1.,8.));
#21912=CARTESIAN_POINT('Origin',(10.3045943951691,-1.,8.));
#21913=CARTESIAN_POINT('',(10.3045943951691,-1.,8.));
#21914=CARTESIAN_POINT('',(10.438768543395,-1.,8.));
#21915=CARTESIAN_POINT('',(10.3045943951691,1.,8.));
#21916=CARTESIAN_POINT('',(10.438768543395,1.,8.));
#21917=CARTESIAN_POINT('',(10.3045943951691,-1.,8.));
#21918=CARTESIAN_POINT('Origin',(10.1408077897493,-1.,8.45));
#21919=CARTESIAN_POINT('',(10.1408077897493,-1.,8.45));
#21920=CARTESIAN_POINT('',(10.3045943951691,-1.,8.));
#21921=CARTESIAN_POINT('',(10.1408077897493,1.,8.45));
#21922=CARTESIAN_POINT('',(10.3045943951691,1.,8.));
#21923=CARTESIAN_POINT('',(10.1408077897493,-1.,8.45));
#21924=CARTESIAN_POINT('Origin',(9.97423661809681,-1.,8.45));
#21925=CARTESIAN_POINT('',(9.97423661809681,-1.,8.45));
#21926=CARTESIAN_POINT('',(10.1408077897493,-1.,8.45));
#21927=CARTESIAN_POINT('',(9.97423661809681,1.,8.45));
#21928=CARTESIAN_POINT('',(10.1408077897493,1.,8.45));
#21929=CARTESIAN_POINT('',(9.97423661809681,-1.,8.45));
#21930=CARTESIAN_POINT('Origin',(9.81045001267702,-1.,8.));
#21931=CARTESIAN_POINT('',(9.81045001267702,-1.,8.));
#21932=CARTESIAN_POINT('',(9.97423661809681,-1.,8.45));
#21933=CARTESIAN_POINT('',(9.81045001267702,1.,8.));
#21934=CARTESIAN_POINT('',(9.97423661809681,1.,8.45));
#21935=CARTESIAN_POINT('',(9.81045001267702,-1.,8.));
#21936=CARTESIAN_POINT('Origin',(9.67627586445114,-1.,8.));
#21937=CARTESIAN_POINT('',(9.67627586445114,-1.,8.));
#21938=CARTESIAN_POINT('',(9.81045001267702,-1.,8.));
#21939=CARTESIAN_POINT('',(9.67627586445114,1.,8.));
#21940=CARTESIAN_POINT('',(9.81045001267702,1.,8.));
#21941=CARTESIAN_POINT('',(9.67627586445114,-1.,8.));
#21942=CARTESIAN_POINT('Origin',(9.51248925903135,-1.,8.45));
#21943=CARTESIAN_POINT('',(9.51248925903135,-1.,8.45));
#21944=CARTESIAN_POINT('',(9.67627586445114,-1.,8.));
#21945=CARTESIAN_POINT('',(9.51248925903135,1.,8.45));
#21946=CARTESIAN_POINT('',(9.67627586445114,1.,8.));
#21947=CARTESIAN_POINT('',(9.51248925903135,-1.,8.45));
#21948=CARTESIAN_POINT('Origin',(9.34591808737885,-1.,8.45));
#21949=CARTESIAN_POINT('',(9.34591808737885,-1.,8.45));
#21950=CARTESIAN_POINT('',(9.51248925903135,-1.,8.45));
#21951=CARTESIAN_POINT('',(9.34591808737885,1.,8.45));
#21952=CARTESIAN_POINT('',(9.51248925903135,1.,8.45));
#21953=CARTESIAN_POINT('',(9.34591808737885,-1.,8.45));
#21954=CARTESIAN_POINT('Origin',(9.18213148195906,-1.,8.));
#21955=CARTESIAN_POINT('',(9.18213148195906,-1.,8.));
#21956=CARTESIAN_POINT('',(9.34591808737885,-1.,8.45));
#21957=CARTESIAN_POINT('',(9.18213148195906,1.,8.));
#21958=CARTESIAN_POINT('',(9.34591808737885,1.,8.45));
#21959=CARTESIAN_POINT('',(9.18213148195906,-1.,8.));
#21960=CARTESIAN_POINT('Origin',(9.04795733373319,-1.,8.));
#21961=CARTESIAN_POINT('',(9.04795733373319,-1.,8.));
#21962=CARTESIAN_POINT('',(9.18213148195906,-1.,8.));
#21963=CARTESIAN_POINT('',(9.04795733373319,1.,8.));
#21964=CARTESIAN_POINT('',(9.18213148195906,1.,8.));
#21965=CARTESIAN_POINT('',(9.04795733373319,-1.,8.));
#21966=CARTESIAN_POINT('Origin',(8.88417072831339,-1.,8.45));
#21967=CARTESIAN_POINT('',(8.88417072831339,-1.,8.45));
#21968=CARTESIAN_POINT('',(9.04795733373319,-1.,8.));
#21969=CARTESIAN_POINT('',(8.88417072831339,1.,8.45));
#21970=CARTESIAN_POINT('',(9.04795733373319,1.,8.));
#21971=CARTESIAN_POINT('',(8.88417072831339,-1.,8.45));
#21972=CARTESIAN_POINT('Origin',(8.7175995566609,-1.,8.45));
#21973=CARTESIAN_POINT('',(8.7175995566609,-1.,8.45));
#21974=CARTESIAN_POINT('',(8.88417072831339,-1.,8.45));
#21975=CARTESIAN_POINT('',(8.7175995566609,1.,8.45));
#21976=CARTESIAN_POINT('',(8.88417072831339,1.,8.45));
#21977=CARTESIAN_POINT('',(8.7175995566609,-1.,8.45));
#21978=CARTESIAN_POINT('Origin',(8.5538129512411,-1.,8.));
#21979=CARTESIAN_POINT('',(8.5538129512411,-1.,8.));
#21980=CARTESIAN_POINT('',(8.7175995566609,-1.,8.45));
#21981=CARTESIAN_POINT('',(8.5538129512411,1.,8.));
#21982=CARTESIAN_POINT('',(8.7175995566609,1.,8.45));
#21983=CARTESIAN_POINT('',(8.5538129512411,-1.,8.));
#21984=CARTESIAN_POINT('Origin',(8.41963880301523,-1.,8.));
#21985=CARTESIAN_POINT('',(8.41963880301523,-1.,8.));
#21986=CARTESIAN_POINT('',(8.5538129512411,-1.,8.));
#21987=CARTESIAN_POINT('',(8.41963880301523,1.,8.));
#21988=CARTESIAN_POINT('',(8.5538129512411,1.,8.));
#21989=CARTESIAN_POINT('',(8.41963880301523,-1.,8.));
#21990=CARTESIAN_POINT('Origin',(8.25585219759544,-1.,8.45));
#21991=CARTESIAN_POINT('',(8.25585219759544,-1.,8.45));
#21992=CARTESIAN_POINT('',(8.41963880301523,-1.,8.));
#21993=CARTESIAN_POINT('',(8.25585219759544,1.,8.45));
#21994=CARTESIAN_POINT('',(8.41963880301523,1.,8.));
#21995=CARTESIAN_POINT('',(8.25585219759544,-1.,8.45));
#21996=CARTESIAN_POINT('Origin',(8.08928102594294,-1.,8.45));
#21997=CARTESIAN_POINT('',(8.08928102594294,-1.,8.45));
#21998=CARTESIAN_POINT('',(8.25585219759544,-1.,8.45));
#21999=CARTESIAN_POINT('',(8.08928102594294,1.,8.45));
#22000=CARTESIAN_POINT('',(8.25585219759544,1.,8.45));
#22001=CARTESIAN_POINT('',(8.08928102594294,-1.,8.45));
#22002=CARTESIAN_POINT('Origin',(7.92549442052315,-1.,8.));
#22003=CARTESIAN_POINT('',(7.92549442052315,-1.,8.));
#22004=CARTESIAN_POINT('',(8.08928102594294,-1.,8.45));
#22005=CARTESIAN_POINT('',(7.92549442052315,1.,8.));
#22006=CARTESIAN_POINT('',(8.08928102594294,1.,8.45));
#22007=CARTESIAN_POINT('',(7.92549442052315,-1.,8.));
#22008=CARTESIAN_POINT('Origin',(7.79132027229727,-1.,8.));
#22009=CARTESIAN_POINT('',(7.79132027229727,-1.,8.));
#22010=CARTESIAN_POINT('',(7.92549442052315,-1.,8.));
#22011=CARTESIAN_POINT('',(7.79132027229727,1.,8.));
#22012=CARTESIAN_POINT('',(7.92549442052315,1.,8.));
#22013=CARTESIAN_POINT('',(7.79132027229727,-1.,8.));
#22014=CARTESIAN_POINT('Origin',(7.62753366687748,-1.,8.45));
#22015=CARTESIAN_POINT('',(7.62753366687748,-1.,8.45));
#22016=CARTESIAN_POINT('',(7.79132027229727,-1.,8.));
#22017=CARTESIAN_POINT('',(7.62753366687748,1.,8.45));
#22018=CARTESIAN_POINT('',(7.79132027229727,1.,8.));
#22019=CARTESIAN_POINT('',(7.62753366687748,-1.,8.45));
#22020=CARTESIAN_POINT('Origin',(7.46096249522498,-1.,8.45));
#22021=CARTESIAN_POINT('',(7.46096249522498,-1.,8.45));
#22022=CARTESIAN_POINT('',(7.62753366687748,-1.,8.45));
#22023=CARTESIAN_POINT('',(7.46096249522498,1.,8.45));
#22024=CARTESIAN_POINT('',(7.62753366687748,1.,8.45));
#22025=CARTESIAN_POINT('',(7.46096249522498,-1.,8.45));
#22026=CARTESIAN_POINT('Origin',(7.29717588980519,-1.,8.));
#22027=CARTESIAN_POINT('',(7.29717588980519,-1.,8.));
#22028=CARTESIAN_POINT('',(7.46096249522498,-1.,8.45));
#22029=CARTESIAN_POINT('',(7.29717588980519,1.,8.));
#22030=CARTESIAN_POINT('',(7.46096249522498,1.,8.45));
#22031=CARTESIAN_POINT('',(7.29717588980519,-1.,8.));
#22032=CARTESIAN_POINT('Origin',(7.16300174157931,-1.,8.));
#22033=CARTESIAN_POINT('',(7.16300174157931,-1.,8.));
#22034=CARTESIAN_POINT('',(7.29717588980519,-1.,8.));
#22035=CARTESIAN_POINT('',(7.16300174157931,1.,8.));
#22036=CARTESIAN_POINT('',(7.29717588980519,1.,8.));
#22037=CARTESIAN_POINT('',(7.16300174157931,-1.,8.));
#22038=CARTESIAN_POINT('Origin',(6.99921513615952,-1.,8.45));
#22039=CARTESIAN_POINT('',(6.99921513615952,-1.,8.45));
#22040=CARTESIAN_POINT('',(7.16300174157931,-1.,8.));
#22041=CARTESIAN_POINT('',(6.99921513615952,1.,8.45));
#22042=CARTESIAN_POINT('',(7.16300174157931,1.,8.));
#22043=CARTESIAN_POINT('',(6.99921513615952,-1.,8.45));
#22044=CARTESIAN_POINT('Origin',(6.83264396450702,-1.,8.45));
#22045=CARTESIAN_POINT('',(6.83264396450702,-1.,8.45));
#22046=CARTESIAN_POINT('',(6.99921513615952,-1.,8.45));
#22047=CARTESIAN_POINT('',(6.83264396450702,1.,8.45));
#22048=CARTESIAN_POINT('',(6.99921513615952,1.,8.45));
#22049=CARTESIAN_POINT('',(6.83264396450702,-1.,8.45));
#22050=CARTESIAN_POINT('Origin',(6.66885735908723,-1.,8.));
#22051=CARTESIAN_POINT('',(6.66885735908723,-1.,8.));
#22052=CARTESIAN_POINT('',(6.83264396450702,-1.,8.45));
#22053=CARTESIAN_POINT('',(6.66885735908723,1.,8.));
#22054=CARTESIAN_POINT('',(6.83264396450702,1.,8.45));
#22055=CARTESIAN_POINT('',(6.66885735908723,-1.,8.));
#22056=CARTESIAN_POINT('Origin',(6.53468321086135,-1.,8.));
#22057=CARTESIAN_POINT('',(6.53468321086135,-1.,8.));
#22058=CARTESIAN_POINT('',(6.66885735908723,-1.,8.));
#22059=CARTESIAN_POINT('',(6.53468321086135,1.,8.));
#22060=CARTESIAN_POINT('',(6.66885735908723,1.,8.));
#22061=CARTESIAN_POINT('',(6.53468321086135,-1.,8.));
#22062=CARTESIAN_POINT('Origin',(6.37089660544156,-1.,8.45));
#22063=CARTESIAN_POINT('',(6.37089660544156,-1.,8.45));
#22064=CARTESIAN_POINT('',(6.53468321086135,-1.,8.));
#22065=CARTESIAN_POINT('',(6.37089660544156,1.,8.45));
#22066=CARTESIAN_POINT('',(6.53468321086135,1.,8.));
#22067=CARTESIAN_POINT('',(6.37089660544156,-1.,8.45));
#22068=CARTESIAN_POINT('Origin',(6.20432543378906,-1.,8.45));
#22069=CARTESIAN_POINT('',(6.20432543378906,-1.,8.45));
#22070=CARTESIAN_POINT('',(6.37089660544156,-1.,8.45));
#22071=CARTESIAN_POINT('',(6.20432543378906,1.,8.45));
#22072=CARTESIAN_POINT('',(6.37089660544156,1.,8.45));
#22073=CARTESIAN_POINT('',(6.20432543378906,-1.,8.45));
#22074=CARTESIAN_POINT('Origin',(6.04053882836927,-1.,8.));
#22075=CARTESIAN_POINT('',(6.04053882836927,-1.,8.));
#22076=CARTESIAN_POINT('',(6.20432543378906,-1.,8.45));
#22077=CARTESIAN_POINT('',(6.04053882836927,1.,8.));
#22078=CARTESIAN_POINT('',(6.20432543378906,1.,8.45));
#22079=CARTESIAN_POINT('',(6.04053882836927,-1.,8.));
#22080=CARTESIAN_POINT('Origin',(5.90636468014339,-1.,8.));
#22081=CARTESIAN_POINT('',(5.90636468014339,-1.,8.));
#22082=CARTESIAN_POINT('',(6.04053882836927,-1.,8.));
#22083=CARTESIAN_POINT('',(5.90636468014339,1.,8.));
#22084=CARTESIAN_POINT('',(6.04053882836927,1.,8.));
#22085=CARTESIAN_POINT('',(5.90636468014339,-1.,8.));
#22086=CARTESIAN_POINT('Origin',(5.7425780747236,-1.,8.45));
#22087=CARTESIAN_POINT('',(5.7425780747236,-1.,8.45));
#22088=CARTESIAN_POINT('',(5.90636468014339,-1.,8.));
#22089=CARTESIAN_POINT('',(5.7425780747236,1.,8.45));
#22090=CARTESIAN_POINT('',(5.90636468014339,1.,8.));
#22091=CARTESIAN_POINT('',(5.7425780747236,-1.,8.45));
#22092=CARTESIAN_POINT('Origin',(5.5760069030711,-1.,8.45));
#22093=CARTESIAN_POINT('',(5.5760069030711,-1.,8.45));
#22094=CARTESIAN_POINT('',(5.7425780747236,-1.,8.45));
#22095=CARTESIAN_POINT('',(5.5760069030711,1.,8.45));
#22096=CARTESIAN_POINT('',(5.7425780747236,1.,8.45));
#22097=CARTESIAN_POINT('',(5.5760069030711,-1.,8.45));
#22098=CARTESIAN_POINT('Origin',(5.41222029765131,-1.,8.));
#22099=CARTESIAN_POINT('',(5.41222029765131,-1.,8.));
#22100=CARTESIAN_POINT('',(5.5760069030711,-1.,8.45));
#22101=CARTESIAN_POINT('',(5.41222029765131,1.,8.));
#22102=CARTESIAN_POINT('',(5.5760069030711,1.,8.45));
#22103=CARTESIAN_POINT('',(5.41222029765131,-1.,8.));
#22104=CARTESIAN_POINT('Origin',(5.27804614942543,-1.,8.));
#22105=CARTESIAN_POINT('',(5.27804614942543,-1.,8.));
#22106=CARTESIAN_POINT('',(5.41222029765131,-1.,8.));
#22107=CARTESIAN_POINT('',(5.27804614942543,1.,8.));
#22108=CARTESIAN_POINT('',(5.41222029765131,1.,8.));
#22109=CARTESIAN_POINT('',(5.27804614942543,-1.,8.));
#22110=CARTESIAN_POINT('Origin',(5.11425954400564,-1.,8.45));
#22111=CARTESIAN_POINT('',(5.11425954400564,-1.,8.45));
#22112=CARTESIAN_POINT('',(5.27804614942543,-1.,8.));
#22113=CARTESIAN_POINT('',(5.11425954400564,1.,8.45));
#22114=CARTESIAN_POINT('',(5.27804614942543,1.,8.));
#22115=CARTESIAN_POINT('',(5.11425954400564,-1.,8.45));
#22116=CARTESIAN_POINT('Origin',(4.94768837235314,-1.,8.45));
#22117=CARTESIAN_POINT('',(4.94768837235314,-1.,8.45));
#22118=CARTESIAN_POINT('',(5.11425954400564,-1.,8.45));
#22119=CARTESIAN_POINT('',(4.94768837235314,1.,8.45));
#22120=CARTESIAN_POINT('',(5.11425954400564,1.,8.45));
#22121=CARTESIAN_POINT('',(4.94768837235314,-1.,8.45));
#22122=CARTESIAN_POINT('Origin',(4.78390176693335,-1.,8.));
#22123=CARTESIAN_POINT('',(4.78390176693335,-1.,8.));
#22124=CARTESIAN_POINT('',(4.94768837235314,-1.,8.45));
#22125=CARTESIAN_POINT('',(4.78390176693335,1.,8.));
#22126=CARTESIAN_POINT('',(4.94768837235314,1.,8.45));
#22127=CARTESIAN_POINT('',(4.78390176693335,-1.,8.));
#22128=CARTESIAN_POINT('Origin',(4.64972761870748,-1.,8.));
#22129=CARTESIAN_POINT('',(4.64972761870748,-1.,8.));
#22130=CARTESIAN_POINT('',(4.78390176693335,-1.,8.));
#22131=CARTESIAN_POINT('',(4.64972761870748,1.,8.));
#22132=CARTESIAN_POINT('',(4.78390176693335,1.,8.));
#22133=CARTESIAN_POINT('',(4.64972761870748,-1.,8.));
#22134=CARTESIAN_POINT('Origin',(4.48594101328768,-1.,8.45));
#22135=CARTESIAN_POINT('',(4.48594101328768,-1.,8.45));
#22136=CARTESIAN_POINT('',(4.64972761870748,-1.,8.));
#22137=CARTESIAN_POINT('',(4.48594101328768,1.,8.45));
#22138=CARTESIAN_POINT('',(4.64972761870748,1.,8.));
#22139=CARTESIAN_POINT('',(4.48594101328768,-1.,8.45));
#22140=CARTESIAN_POINT('Origin',(4.31936984163519,-1.,8.45));
#22141=CARTESIAN_POINT('',(4.31936984163519,-1.,8.45));
#22142=CARTESIAN_POINT('',(4.48594101328768,-1.,8.45));
#22143=CARTESIAN_POINT('',(4.31936984163519,1.,8.45));
#22144=CARTESIAN_POINT('',(4.48594101328768,1.,8.45));
#22145=CARTESIAN_POINT('',(4.31936984163519,-1.,8.45));
#22146=CARTESIAN_POINT('Origin',(4.15558323621539,-1.,8.));
#22147=CARTESIAN_POINT('',(4.15558323621539,-1.,8.));
#22148=CARTESIAN_POINT('',(4.31936984163519,-1.,8.45));
#22149=CARTESIAN_POINT('',(4.15558323621539,1.,8.));
#22150=CARTESIAN_POINT('',(4.31936984163519,1.,8.45));
#22151=CARTESIAN_POINT('',(4.15558323621539,-1.,8.));
#22152=CARTESIAN_POINT('Origin',(4.02140908798952,-1.,8.));
#22153=CARTESIAN_POINT('',(4.02140908798952,-1.,8.));
#22154=CARTESIAN_POINT('',(4.15558323621539,-1.,8.));
#22155=CARTESIAN_POINT('',(4.02140908798952,1.,8.));
#22156=CARTESIAN_POINT('',(4.15558323621539,1.,8.));
#22157=CARTESIAN_POINT('',(4.02140908798952,-1.,8.));
#22158=CARTESIAN_POINT('Origin',(3.85762248256973,-1.,8.45));
#22159=CARTESIAN_POINT('',(3.85762248256973,-1.,8.45));
#22160=CARTESIAN_POINT('',(4.02140908798952,-1.,8.));
#22161=CARTESIAN_POINT('',(3.85762248256973,1.,8.45));
#22162=CARTESIAN_POINT('',(4.02140908798952,1.,8.));
#22163=CARTESIAN_POINT('',(3.85762248256973,-1.,8.45));
#22164=CARTESIAN_POINT('Origin',(3.69105131091723,-1.,8.45));
#22165=CARTESIAN_POINT('',(3.69105131091723,-1.,8.45));
#22166=CARTESIAN_POINT('',(3.85762248256973,-1.,8.45));
#22167=CARTESIAN_POINT('',(3.69105131091723,1.,8.45));
#22168=CARTESIAN_POINT('',(3.85762248256973,1.,8.45));
#22169=CARTESIAN_POINT('',(3.69105131091723,-1.,8.45));
#22170=CARTESIAN_POINT('Origin',(3.52726470549744,-1.,8.));
#22171=CARTESIAN_POINT('',(3.52726470549744,-1.,8.));
#22172=CARTESIAN_POINT('',(3.69105131091723,-1.,8.45));
#22173=CARTESIAN_POINT('',(3.52726470549744,1.,8.));
#22174=CARTESIAN_POINT('',(3.69105131091723,1.,8.45));
#22175=CARTESIAN_POINT('',(3.52726470549744,-1.,8.));
#22176=CARTESIAN_POINT('Origin',(3.39309055727156,-1.,8.));
#22177=CARTESIAN_POINT('',(3.39309055727156,-1.,8.));
#22178=CARTESIAN_POINT('',(3.52726470549744,-1.,8.));
#22179=CARTESIAN_POINT('',(3.39309055727156,1.,8.));
#22180=CARTESIAN_POINT('',(3.52726470549744,1.,8.));
#22181=CARTESIAN_POINT('',(3.39309055727156,-1.,8.));
#22182=CARTESIAN_POINT('Origin',(3.22930395185177,-1.,8.45));
#22183=CARTESIAN_POINT('',(3.22930395185177,-1.,8.45));
#22184=CARTESIAN_POINT('',(3.39309055727156,-1.,8.));
#22185=CARTESIAN_POINT('',(3.22930395185177,1.,8.45));
#22186=CARTESIAN_POINT('',(3.39309055727156,1.,8.));
#22187=CARTESIAN_POINT('',(3.22930395185177,-1.,8.45));
#22188=CARTESIAN_POINT('Origin',(3.06273278019927,-1.,8.45));
#22189=CARTESIAN_POINT('',(3.06273278019927,-1.,8.45));
#22190=CARTESIAN_POINT('',(3.22930395185177,-1.,8.45));
#22191=CARTESIAN_POINT('',(3.06273278019927,1.,8.45));
#22192=CARTESIAN_POINT('',(3.22930395185177,1.,8.45));
#22193=CARTESIAN_POINT('',(3.06273278019927,-1.,8.45));
#22194=CARTESIAN_POINT('Origin',(2.89894617477948,-1.,8.));
#22195=CARTESIAN_POINT('',(2.89894617477948,-1.,8.));
#22196=CARTESIAN_POINT('',(3.06273278019927,-1.,8.45));
#22197=CARTESIAN_POINT('',(2.89894617477948,1.,8.));
#22198=CARTESIAN_POINT('',(3.06273278019927,1.,8.45));
#22199=CARTESIAN_POINT('',(2.89894617477948,-1.,8.));
#22200=CARTESIAN_POINT('Origin',(2.7647720265536,-1.,8.));
#22201=CARTESIAN_POINT('',(2.7647720265536,-1.,8.));
#22202=CARTESIAN_POINT('',(2.89894617477948,-1.,8.));
#22203=CARTESIAN_POINT('',(2.7647720265536,1.,8.));
#22204=CARTESIAN_POINT('',(2.89894617477948,1.,8.));
#22205=CARTESIAN_POINT('',(2.7647720265536,-1.,8.));
#22206=CARTESIAN_POINT('Origin',(2.60098542113381,-1.,8.45));
#22207=CARTESIAN_POINT('',(2.60098542113381,-1.,8.45));
#22208=CARTESIAN_POINT('',(2.7647720265536,-1.,8.));
#22209=CARTESIAN_POINT('',(2.60098542113381,1.,8.45));
#22210=CARTESIAN_POINT('',(2.7647720265536,1.,8.));
#22211=CARTESIAN_POINT('',(2.60098542113381,-1.,8.45));
#22212=CARTESIAN_POINT('Origin',(2.43441424948131,-1.,8.45));
#22213=CARTESIAN_POINT('',(2.43441424948131,-1.,8.45));
#22214=CARTESIAN_POINT('',(2.60098542113381,-1.,8.45));
#22215=CARTESIAN_POINT('',(2.43441424948131,1.,8.45));
#22216=CARTESIAN_POINT('',(2.60098542113381,1.,8.45));
#22217=CARTESIAN_POINT('',(2.43441424948131,-1.,8.45));
#22218=CARTESIAN_POINT('Origin',(2.27062764406152,-1.,8.));
#22219=CARTESIAN_POINT('',(2.27062764406152,-1.,8.));
#22220=CARTESIAN_POINT('',(2.43441424948131,-1.,8.45));
#22221=CARTESIAN_POINT('',(2.27062764406152,1.,8.));
#22222=CARTESIAN_POINT('',(2.43441424948131,1.,8.45));
#22223=CARTESIAN_POINT('',(2.27062764406152,-1.,8.));
#22224=CARTESIAN_POINT('Origin',(2.13645349583564,-1.,8.));
#22225=CARTESIAN_POINT('',(2.13645349583564,-1.,8.));
#22226=CARTESIAN_POINT('',(2.27062764406152,-1.,8.));
#22227=CARTESIAN_POINT('',(2.13645349583564,1.,8.));
#22228=CARTESIAN_POINT('',(2.27062764406152,1.,8.));
#22229=CARTESIAN_POINT('',(2.13645349583564,-1.,8.));
#22230=CARTESIAN_POINT('Origin',(1.97266689041585,-1.,8.45));
#22231=CARTESIAN_POINT('',(1.97266689041585,-1.,8.45));
#22232=CARTESIAN_POINT('',(2.13645349583564,-1.,8.));
#22233=CARTESIAN_POINT('',(1.97266689041585,1.,8.45));
#22234=CARTESIAN_POINT('',(2.13645349583564,1.,8.));
#22235=CARTESIAN_POINT('',(1.97266689041585,-1.,8.45));
#22236=CARTESIAN_POINT('Origin',(1.80609571876335,-1.,8.45));
#22237=CARTESIAN_POINT('',(1.80609571876335,-1.,8.45));
#22238=CARTESIAN_POINT('',(1.97266689041585,-1.,8.45));
#22239=CARTESIAN_POINT('',(1.80609571876335,1.,8.45));
#22240=CARTESIAN_POINT('',(1.97266689041585,1.,8.45));
#22241=CARTESIAN_POINT('',(1.80609571876335,-1.,8.45));
#22242=CARTESIAN_POINT('Origin',(1.64230911334356,-1.,8.));
#22243=CARTESIAN_POINT('',(1.64230911334356,-1.,8.));
#22244=CARTESIAN_POINT('',(1.80609571876335,-1.,8.45));
#22245=CARTESIAN_POINT('',(1.64230911334356,1.,8.));
#22246=CARTESIAN_POINT('',(1.80609571876335,1.,8.45));
#22247=CARTESIAN_POINT('',(1.64230911334356,-1.,8.));
#22248=CARTESIAN_POINT('Origin',(1.,-1.,8.));
#22249=CARTESIAN_POINT('',(1.64230911334356,-1.,8.));
#22250=CARTESIAN_POINT('',(1.64230911334356,1.,8.));
#22251=CARTESIAN_POINT('Origin',(11.,1.,7.725));
#22252=CARTESIAN_POINT('Origin',(11.,-1.,7.725));
#22253=CARTESIAN_POINT('',(0.,0.,0.));
#22254=CARTESIAN_POINT('',(0.,0.,0.));
#22255=CARTESIAN_POINT('Origin',(1.5,-1.9,1.7));
#22256=CARTESIAN_POINT('',(1.56403124237433,-1.7,1.7));
#22257=CARTESIAN_POINT('',(1.43596875762567,-1.7,1.7));
#22258=CARTESIAN_POINT('',(0.75,-1.7,1.7));
#22259=CARTESIAN_POINT('Origin',(1.5,-1.9,1.7));
#22260=CARTESIAN_POINT('Origin',(1.5,-1.9,1.7));
#22261=CARTESIAN_POINT('',(1.56403124237433,-1.7,1.75));
#22262=CARTESIAN_POINT('',(1.56403124237433,-1.7,1.7));
#22263=CARTESIAN_POINT('',(1.29,-1.9,1.75));
#22264=CARTESIAN_POINT('Origin',(1.5,-1.9,1.75));
#22265=CARTESIAN_POINT('',(1.29,-1.9,2.4));
#22266=CARTESIAN_POINT('',(1.29,-1.9,1.7));
#22267=CARTESIAN_POINT('Origin',(1.5,-1.9,2.4));
#22268=CARTESIAN_POINT('',(1.43596875762567,-1.7,1.75));
#22269=CARTESIAN_POINT('Origin',(1.5,-1.9,1.75));
#22270=CARTESIAN_POINT('',(1.43596875762567,-1.7,1.7));
#22271=CARTESIAN_POINT('Origin',(-1.5,1.9,1.7));
#22272=CARTESIAN_POINT('',(-1.56403124237433,1.7,1.7));
#22273=CARTESIAN_POINT('',(-1.43596875762567,1.7,1.7));
#22274=CARTESIAN_POINT('',(-0.75,1.7,1.7));
#22275=CARTESIAN_POINT('Origin',(-1.5,1.9,1.7));
#22276=CARTESIAN_POINT('Origin',(-1.5,1.9,1.7));
#22277=CARTESIAN_POINT('',(-1.56403124237433,1.7,1.75));
#22278=CARTESIAN_POINT('',(-1.56403124237433,1.7,1.7));
#22279=CARTESIAN_POINT('',(-1.71,1.9,1.75));
#22280=CARTESIAN_POINT('Origin',(-1.5,1.9,1.75));
#22281=CARTESIAN_POINT('',(-1.71,1.9,2.4));
#22282=CARTESIAN_POINT('',(-1.71,1.9,1.7));
#22283=CARTESIAN_POINT('Origin',(-1.5,1.9,2.4));
#22284=CARTESIAN_POINT('',(-1.43596875762567,1.7,1.75));
#22285=CARTESIAN_POINT('Origin',(-1.5,1.9,1.75));
#22286=CARTESIAN_POINT('',(-1.43596875762567,1.7,1.7));
#22287=CARTESIAN_POINT('Origin',(-1.5,-1.9,1.7));
#22288=CARTESIAN_POINT('',(-1.43596875762567,-1.7,1.7));
#22289=CARTESIAN_POINT('',(-1.56403124237433,-1.7,1.7));
#22290=CARTESIAN_POINT('',(-0.75,-1.7,1.7));
#22291=CARTESIAN_POINT('Origin',(-1.5,-1.9,1.7));
#22292=CARTESIAN_POINT('Origin',(-1.5,-1.9,1.7));
#22293=CARTESIAN_POINT('',(-1.43596875762567,-1.7,1.75));
#22294=CARTESIAN_POINT('',(-1.43596875762567,-1.7,1.7));
#22295=CARTESIAN_POINT('',(-1.71,-1.9,1.75));
#22296=CARTESIAN_POINT('Origin',(-1.5,-1.9,1.75));
#22297=CARTESIAN_POINT('',(-1.71,-1.9,2.4));
#22298=CARTESIAN_POINT('',(-1.71,-1.9,1.7));
#22299=CARTESIAN_POINT('Origin',(-1.5,-1.9,2.4));
#22300=CARTESIAN_POINT('',(-1.56403124237433,-1.7,1.75));
#22301=CARTESIAN_POINT('Origin',(-1.5,-1.9,1.75));
#22302=CARTESIAN_POINT('',(-1.56403124237433,-1.7,1.7));
#22303=CARTESIAN_POINT('Origin',(1.5,1.9,1.7));
#22304=CARTESIAN_POINT('',(1.43596875762567,1.7,1.7));
#22305=CARTESIAN_POINT('',(1.56403124237433,1.7,1.7));
#22306=CARTESIAN_POINT('',(0.75,1.7,1.7));
#22307=CARTESIAN_POINT('Origin',(1.5,1.9,1.7));
#22308=CARTESIAN_POINT('Origin',(1.5,1.9,1.7));
#22309=CARTESIAN_POINT('',(1.43596875762567,1.7,1.75));
#22310=CARTESIAN_POINT('',(1.43596875762567,1.7,1.7));
#22311=CARTESIAN_POINT('',(1.29,1.9,1.75));
#22312=CARTESIAN_POINT('Origin',(1.5,1.9,1.75));
#22313=CARTESIAN_POINT('',(1.29,1.9,2.4));
#22314=CARTESIAN_POINT('',(1.29,1.9,1.7));
#22315=CARTESIAN_POINT('Origin',(1.5,1.9,2.4));
#22316=CARTESIAN_POINT('',(1.56403124237433,1.7,1.75));
#22317=CARTESIAN_POINT('Origin',(1.5,1.9,1.75));
#22318=CARTESIAN_POINT('',(1.56403124237433,1.7,1.7));
#22319=CARTESIAN_POINT('Origin',(0.,-1.7,1.75));
#22320=CARTESIAN_POINT('',(0.,-1.7,1.75));
#22321=CARTESIAN_POINT('',(-1.97,-1.7,1.75));
#22322=CARTESIAN_POINT('',(0.,-1.7,1.75));
#22323=CARTESIAN_POINT('',(-1.97,-1.7,0.43));
#22324=CARTESIAN_POINT('',(-1.97,-1.7,1.75));
#22325=CARTESIAN_POINT('',(1.97,-1.7,0.43));
#22326=CARTESIAN_POINT('',(0.,-1.7,0.43));
#22327=CARTESIAN_POINT('',(1.97,-1.7,1.75));
#22328=CARTESIAN_POINT('',(1.97,-1.7,1.75));
#22329=CARTESIAN_POINT('',(0.,-1.7,1.75));
#22330=CARTESIAN_POINT('Origin',(0.,1.7,0.43));
#22331=CARTESIAN_POINT('',(0.,1.7,1.75));
#22332=CARTESIAN_POINT('',(1.97,1.7,1.75));
#22333=CARTESIAN_POINT('',(0.,1.7,1.75));
#22334=CARTESIAN_POINT('',(1.97,1.7,0.43));
#22335=CARTESIAN_POINT('',(1.97,1.7,0.43));
#22336=CARTESIAN_POINT('',(-1.97,1.7,0.43));
#22337=CARTESIAN_POINT('',(0.,1.7,0.43));
#22338=CARTESIAN_POINT('',(-1.97,1.7,1.75));
#22339=CARTESIAN_POINT('',(-1.97,1.7,0.43));
#22340=CARTESIAN_POINT('',(0.,1.7,1.75));
#22341=CARTESIAN_POINT('Origin',(-1.97,0.,1.415));
#22342=CARTESIAN_POINT('',(-1.97,-2.35,1.75));
#22343=CARTESIAN_POINT('',(-1.97,-2.35,1.75));
#22344=CARTESIAN_POINT('',(-1.97,-2.35,2.4));
#22345=CARTESIAN_POINT('',(-1.97,-2.35,2.4));
#22346=CARTESIAN_POINT('',(-1.97,2.35,2.4));
#22347=CARTESIAN_POINT('',(-1.97,2.35,2.4));
#22348=CARTESIAN_POINT('',(-1.97,2.35,1.75));
#22349=CARTESIAN_POINT('',(-1.97,2.35,1.75));
#22350=CARTESIAN_POINT('',(-1.97,1.7,1.75));
#22351=CARTESIAN_POINT('',(-1.97,0.78,0.43));
#22352=CARTESIAN_POINT('',(-1.97,0.78,0.43));
#22353=CARTESIAN_POINT('',(-1.97,0.78,1.55));
#22354=CARTESIAN_POINT('',(-1.97,0.78,1.55));
#22355=CARTESIAN_POINT('',(-1.97,-0.78,1.55));
#22356=CARTESIAN_POINT('',(-1.97,-0.78,1.55));
#22357=CARTESIAN_POINT('',(-1.97,-0.78,0.43));
#22358=CARTESIAN_POINT('',(-1.97,-0.78,0.43));
#22359=CARTESIAN_POINT('',(-1.97,-1.7,0.43));
#22360=CARTESIAN_POINT('Origin',(0.,-2.35,1.75));
#22361=CARTESIAN_POINT('',(1.97,-2.35,1.75));
#22362=CARTESIAN_POINT('',(1.97,-2.35,1.75));
#22363=CARTESIAN_POINT('',(0.,-2.35,1.75));
#22364=CARTESIAN_POINT('Origin',(0.,-2.35,2.4));
#22365=CARTESIAN_POINT('',(1.97,-2.35,2.4));
#22366=CARTESIAN_POINT('',(1.97,-2.35,2.4));
#22367=CARTESIAN_POINT('',(0.,-2.35,2.4));
#22368=CARTESIAN_POINT('Origin',(0.,2.35,2.4));
#22369=CARTESIAN_POINT('',(1.97,2.35,2.4));
#22370=CARTESIAN_POINT('',(1.97,2.35,2.4));
#22371=CARTESIAN_POINT('',(0.,2.35,2.4));
#22372=CARTESIAN_POINT('Origin',(0.,2.35,1.75));
#22373=CARTESIAN_POINT('',(1.97,2.35,1.75));
#22374=CARTESIAN_POINT('',(1.97,2.35,1.75));
#22375=CARTESIAN_POINT('',(0.,2.35,1.75));
#22376=CARTESIAN_POINT('Origin',(0.,1.7,1.75));
#22377=CARTESIAN_POINT('',(1.97,1.7,1.75));
#22378=CARTESIAN_POINT('Origin',(0.,0.78,0.43));
#22379=CARTESIAN_POINT('',(1.97,0.78,0.43));
#22380=CARTESIAN_POINT('',(1.97,0.78,0.43));
#22381=CARTESIAN_POINT('',(0.,0.78,0.43));
#22382=CARTESIAN_POINT('Origin',(0.,0.78,1.55));
#22383=CARTESIAN_POINT('',(1.97,0.78,1.55));
#22384=CARTESIAN_POINT('',(1.97,0.78,1.55));
#22385=CARTESIAN_POINT('',(0.,0.78,1.55));
#22386=CARTESIAN_POINT('Origin',(0.,-0.78,1.55));
#22387=CARTESIAN_POINT('',(1.97,-0.78,1.55));
#22388=CARTESIAN_POINT('',(1.97,-0.78,1.55));
#22389=CARTESIAN_POINT('',(0.,-0.78,1.55));
#22390=CARTESIAN_POINT('Origin',(0.,-0.78,0.43));
#22391=CARTESIAN_POINT('',(1.97,-0.78,0.43));
#22392=CARTESIAN_POINT('',(1.97,-0.78,0.43));
#22393=CARTESIAN_POINT('',(0.,-0.78,0.43));
#22394=CARTESIAN_POINT('Origin',(0.,-1.7,0.43));
#22395=CARTESIAN_POINT('',(1.97,-1.7,0.43));
#22396=CARTESIAN_POINT('Origin',(1.97,0.,1.415));
#22397=CARTESIAN_POINT('',(0.,0.,0.));
#22398=CARTESIAN_POINT('Origin',(1.97,1.7,2.3));
#22399=CARTESIAN_POINT('',(1.97,1.7,2.3));
#22400=CARTESIAN_POINT('',(1.97,-1.7,2.3));
#22401=CARTESIAN_POINT('',(1.97,1.7,2.3));
#22402=CARTESIAN_POINT('',(3.07,-1.7,2.3));
#22403=CARTESIAN_POINT('',(1.97,-1.7,2.3));
#22404=CARTESIAN_POINT('',(3.07,1.7,2.3));
#22405=CARTESIAN_POINT('',(3.07,1.7,2.3));
#22406=CARTESIAN_POINT('',(1.97,1.7,2.3));
#22407=CARTESIAN_POINT('Origin',(1.97,1.7,0.46));
#22408=CARTESIAN_POINT('',(1.97,1.7,0.46));
#22409=CARTESIAN_POINT('',(1.97,1.7,0.46));
#22410=CARTESIAN_POINT('',(3.07,1.7,0.46));
#22411=CARTESIAN_POINT('',(3.07,1.7,0.46));
#22412=CARTESIAN_POINT('',(1.97,1.7,0.46));
#22413=CARTESIAN_POINT('Origin',(1.97,0.78,0.46));
#22414=CARTESIAN_POINT('',(1.97,0.78,0.46));
#22415=CARTESIAN_POINT('',(1.97,0.78,0.46));
#22416=CARTESIAN_POINT('',(3.07,0.78,0.46));
#22417=CARTESIAN_POINT('',(3.07,0.78,0.46));
#22418=CARTESIAN_POINT('',(1.97,0.78,0.46));
#22419=CARTESIAN_POINT('Origin',(1.97,0.78,1.55));
#22420=CARTESIAN_POINT('',(1.97,0.78,1.55));
#22421=CARTESIAN_POINT('',(1.97,0.78,1.55));
#22422=CARTESIAN_POINT('',(3.07,0.78,1.55));
#22423=CARTESIAN_POINT('',(3.07,0.78,1.55));
#22424=CARTESIAN_POINT('',(1.97,0.78,1.55));
#22425=CARTESIAN_POINT('Origin',(1.97,-0.78,1.55));
#22426=CARTESIAN_POINT('',(1.97,-0.78,1.55));
#22427=CARTESIAN_POINT('',(1.97,-0.78,1.55));
#22428=CARTESIAN_POINT('',(3.07,-0.78,1.55));
#22429=CARTESIAN_POINT('',(3.07,-0.78,1.55));
#22430=CARTESIAN_POINT('',(1.97,-0.78,1.55));
#22431=CARTESIAN_POINT('Origin',(1.97,-0.78,0.46));
#22432=CARTESIAN_POINT('',(1.97,-0.78,0.46));
#22433=CARTESIAN_POINT('',(1.97,-0.78,0.46));
#22434=CARTESIAN_POINT('',(3.07,-0.78,0.46));
#22435=CARTESIAN_POINT('',(3.07,-0.78,0.46));
#22436=CARTESIAN_POINT('',(1.97,-0.78,0.46));
#22437=CARTESIAN_POINT('Origin',(1.97,-1.7,0.46));
#22438=CARTESIAN_POINT('',(1.97,-1.7,0.46));
#22439=CARTESIAN_POINT('',(1.97,-1.7,0.46));
#22440=CARTESIAN_POINT('',(3.07,-1.7,0.46));
#22441=CARTESIAN_POINT('',(3.07,-1.7,0.46));
#22442=CARTESIAN_POINT('',(1.97,-1.7,0.46));
#22443=CARTESIAN_POINT('Origin',(1.97,-1.7,2.3));
#22444=CARTESIAN_POINT('',(1.97,-1.7,2.3));
#22445=CARTESIAN_POINT('',(3.07,-1.7,2.3));
#22446=CARTESIAN_POINT('Origin',(3.07,0.,1.38));
#22447=CARTESIAN_POINT('Origin',(1.97,0.,1.38));
#22448=CARTESIAN_POINT('',(0.,0.,0.));
#22449=CARTESIAN_POINT('Origin',(-1.97,-0.78,0.46));
#22450=CARTESIAN_POINT('',(-1.97,-1.7,0.46));
#22451=CARTESIAN_POINT('',(-1.97,-0.78,0.46));
#22452=CARTESIAN_POINT('',(-1.97,-1.7,0.46));
#22453=CARTESIAN_POINT('',(-3.07,-1.7,0.46));
#22454=CARTESIAN_POINT('',(-1.97,-1.7,0.46));
#22455=CARTESIAN_POINT('',(-3.07,-0.78,0.46));
#22456=CARTESIAN_POINT('',(-3.07,-1.7,0.46));
#22457=CARTESIAN_POINT('',(-1.97,-0.78,0.46));
#22458=CARTESIAN_POINT('Origin',(-1.97,-0.78,1.55));
#22459=CARTESIAN_POINT('',(-1.97,-0.78,1.55));
#22460=CARTESIAN_POINT('',(-1.97,-0.78,0.46));
#22461=CARTESIAN_POINT('',(-3.07,-0.78,1.55));
#22462=CARTESIAN_POINT('',(-3.07,-0.78,0.46));
#22463=CARTESIAN_POINT('',(-1.97,-0.78,1.55));
#22464=CARTESIAN_POINT('Origin',(-1.97,0.78,1.55));
#22465=CARTESIAN_POINT('',(-1.97,0.78,1.55));
#22466=CARTESIAN_POINT('',(-1.97,-0.78,1.55));
#22467=CARTESIAN_POINT('',(-3.07,0.78,1.55));
#22468=CARTESIAN_POINT('',(-3.07,-0.78,1.55));
#22469=CARTESIAN_POINT('',(-1.97,0.78,1.55));
#22470=CARTESIAN_POINT('Origin',(-1.97,0.78,0.46));
#22471=CARTESIAN_POINT('',(-1.97,0.78,0.46));
#22472=CARTESIAN_POINT('',(-1.97,0.78,1.55));
#22473=CARTESIAN_POINT('',(-3.07,0.78,0.46));
#22474=CARTESIAN_POINT('',(-3.07,0.78,1.55));
#22475=CARTESIAN_POINT('',(-1.97,0.78,0.46));
#22476=CARTESIAN_POINT('Origin',(-1.97,1.7,0.46));
#22477=CARTESIAN_POINT('',(-1.97,1.7,0.46));
#22478=CARTESIAN_POINT('',(-1.97,0.78,0.46));
#22479=CARTESIAN_POINT('',(-3.07,1.7,0.46));
#22480=CARTESIAN_POINT('',(-3.07,0.78,0.46));
#22481=CARTESIAN_POINT('',(-1.97,1.7,0.46));
#22482=CARTESIAN_POINT('Origin',(-1.97,1.7,2.3));
#22483=CARTESIAN_POINT('',(-1.97,1.7,2.3));
#22484=CARTESIAN_POINT('',(-1.97,1.7,0.46));
#22485=CARTESIAN_POINT('',(-3.07,1.7,2.3));
#22486=CARTESIAN_POINT('',(-3.07,1.7,0.46));
#22487=CARTESIAN_POINT('',(-1.97,1.7,2.3));
#22488=CARTESIAN_POINT('Origin',(-1.97,-1.7,2.3));
#22489=CARTESIAN_POINT('',(-1.97,-1.7,2.3));
#22490=CARTESIAN_POINT('',(-1.97,1.7,2.3));
#22491=CARTESIAN_POINT('',(-3.07,-1.7,2.3));
#22492=CARTESIAN_POINT('',(-3.07,1.7,2.3));
#22493=CARTESIAN_POINT('',(-1.97,-1.7,2.3));
#22494=CARTESIAN_POINT('Origin',(-1.97,-1.7,0.46));
#22495=CARTESIAN_POINT('',(-1.97,-1.7,2.3));
#22496=CARTESIAN_POINT('',(-3.07,-1.7,2.3));
#22497=CARTESIAN_POINT('Origin',(-1.97,0.,1.38));
#22498=CARTESIAN_POINT('Origin',(-3.07,0.,1.38));
#22499=CARTESIAN_POINT('',(0.,0.,0.));
#22500=CARTESIAN_POINT('',(0.,0.,0.));
#22501=CARTESIAN_POINT('',(0.,0.,0.));
#22502=CARTESIAN_POINT('',(0.,0.,0.));
#22503=CARTESIAN_POINT('Origin',(0.115470053837925,-0.5,-0.2));
#22504=CARTESIAN_POINT('',(0.23094010767585,-0.5,0.));
#22505=CARTESIAN_POINT('',(0.115470053837925,-0.5,-0.2));
#22506=CARTESIAN_POINT('',(0.23094010767585,-0.5,0.));
#22507=CARTESIAN_POINT('',(0.115470053837925,-0.8,-0.2));
#22508=CARTESIAN_POINT('',(0.115470053837925,-0.5,-0.2));
#22509=CARTESIAN_POINT('',(0.23094010767585,-0.8,0.));
#22510=CARTESIAN_POINT('',(0.23094010767585,-0.8,0.));
#22511=CARTESIAN_POINT('',(0.23094010767585,-0.5,0.));
#22512=CARTESIAN_POINT('Origin',(-0.115470053837925,-0.5,-0.2));
#22513=CARTESIAN_POINT('',(-0.115470053837925,-0.5,-0.2));
#22514=CARTESIAN_POINT('',(0.115470053837925,-0.5,-0.2));
#22515=CARTESIAN_POINT('',(-0.115470053837925,-0.8,-0.2));
#22516=CARTESIAN_POINT('',(-0.115470053837925,-0.5,-0.2));
#22517=CARTESIAN_POINT('',(0.115470053837925,-0.8,-0.2));
#22518=CARTESIAN_POINT('Origin',(-0.23094010767585,-0.5,-2.77555756156289E-17));
#22519=CARTESIAN_POINT('',(-0.23094010767585,-0.5,-2.82820063659975E-17));
#22520=CARTESIAN_POINT('',(-0.115470053837925,-0.5,-0.2));
#22521=CARTESIAN_POINT('',(-0.23094010767585,-0.8,-2.77555756156289E-17));
#22522=CARTESIAN_POINT('',(-0.23094010767585,-0.5,-2.82820063659975E-17));
#22523=CARTESIAN_POINT('',(-0.115470053837925,-0.8,-0.2));
#22524=CARTESIAN_POINT('Origin',(-0.115470053837925,-0.5,0.2));
#22525=CARTESIAN_POINT('',(-0.115470053837925,-0.5,0.2));
#22526=CARTESIAN_POINT('',(-0.23094010767585,-0.5,-2.82820063659975E-17));
#22527=CARTESIAN_POINT('',(-0.115470053837925,-0.8,0.2));
#22528=CARTESIAN_POINT('',(-0.115470053837925,-0.5,0.2));
#22529=CARTESIAN_POINT('',(-0.23094010767585,-0.8,-2.82820063659975E-17));
#22530=CARTESIAN_POINT('Origin',(0.115470053837925,-0.5,0.2));
#22531=CARTESIAN_POINT('',(0.115470053837925,-0.5,0.2));
#22532=CARTESIAN_POINT('',(-0.115470053837925,-0.5,0.2));
#22533=CARTESIAN_POINT('',(0.115470053837925,-0.8,0.2));
#22534=CARTESIAN_POINT('',(0.115470053837925,-0.5,0.2));
#22535=CARTESIAN_POINT('',(-0.115470053837925,-0.8,0.2));
#22536=CARTESIAN_POINT('Origin',(0.23094010767585,-0.5,0.));
#22537=CARTESIAN_POINT('',(0.115470053837925,-0.5,0.2));
#22538=CARTESIAN_POINT('',(0.115470053837925,-0.8,0.2));
#22539=CARTESIAN_POINT('Origin',(0.,-0.5,0.));
#22540=CARTESIAN_POINT('Origin',(0.,-0.8,0.));
#22541=CARTESIAN_POINT('Origin',(0.,-1.4,0.));
#22542=CARTESIAN_POINT('',(-0.24505,-1.4,3.00099698131059E-17));
#22543=CARTESIAN_POINT('Origin',(0.,-1.4,0.));
#22544=CARTESIAN_POINT('Origin',(0.375,0.5,0.));
#22545=CARTESIAN_POINT('',(-0.375,0.5,-4.59242549680257E-17));
#22546=CARTESIAN_POINT('Origin',(0.,0.5,0.));
#22547=CARTESIAN_POINT('Origin',(0.,0.475,0.));
#22548=CARTESIAN_POINT('',(-0.425,0.45,-5.20474889637625E-17));
#22549=CARTESIAN_POINT('Origin',(0.,0.45,0.));
#22550=CARTESIAN_POINT('',(-0.4,0.475,-4.89858719658941E-17));
#22551=CARTESIAN_POINT('Origin',(0.,0.24,0.));
#22552=CARTESIAN_POINT('',(-0.425,0.0299999999999998,-5.20474889637625E-17));
#22553=CARTESIAN_POINT('Origin',(0.,0.0299999999999998,0.));
#22554=CARTESIAN_POINT('',(-0.425,0.24,-5.20474889637625E-17));
#22555=CARTESIAN_POINT('Origin',(0.,0.0150000000000001,0.));
#22556=CARTESIAN_POINT('',(-0.395,4.85722573273506E-17,-4.83735485663204E-17));
#22557=CARTESIAN_POINT('Origin',(0.,0.,0.));
#22558=CARTESIAN_POINT('',(-0.41,0.0150000000000001,-5.02105187650415E-17));
#22559=CARTESIAN_POINT('Origin',(0.27,0.,0.));
#22560=CARTESIAN_POINT('',(-0.27,0.,-3.30654635769785E-17));
#22561=CARTESIAN_POINT('Origin',(0.,0.,0.));
#22562=CARTESIAN_POINT('Origin',(0.,-0.02,0.));
#22563=CARTESIAN_POINT('',(-0.24505,-0.0498999999999999,3.00099698131059E-17));
#22564=CARTESIAN_POINT('Origin',(0.,-0.0498999999999999,0.));
#22565=CARTESIAN_POINT('',(-0.26,-0.02,-3.18408167778312E-17));
#22566=CARTESIAN_POINT('Origin',(0.,-0.995,0.));
#22567=CARTESIAN_POINT('',(-0.24505,-0.995,-3.00099698131059E-17));
#22568=CARTESIAN_POINT('',(0.,0.,0.));
#22569=CARTESIAN_POINT('',(0.,0.,0.));
#22570=CARTESIAN_POINT('Origin',(10.8,6.2,9.55));
#22571=CARTESIAN_POINT('',(10.8,7.6,9.68431457505076));
#22572=CARTESIAN_POINT('',(10.8,6.2,9.68431457505076));
#22573=CARTESIAN_POINT('',(10.8,-6.5,9.68431457505076));
#22574=CARTESIAN_POINT('',(10.8,7.6,9.9));
#22575=CARTESIAN_POINT('',(10.8,7.6,9.9));
#22576=CARTESIAN_POINT('',(10.8,6.2,9.9));
#22577=CARTESIAN_POINT('',(10.8,6.2,9.9));
#22578=CARTESIAN_POINT('',(10.8,6.2,9.9));
#22579=CARTESIAN_POINT('Origin',(11.,6.2,9.725));
#22580=CARTESIAN_POINT('',(11.2,6.2,9.68431457505076));
#22581=CARTESIAN_POINT('Origin',(11.,6.2,10.25));
#22582=CARTESIAN_POINT('',(11.2,6.2,9.9));
#22583=CARTESIAN_POINT('',(11.2,6.2,9.9));
#22584=CARTESIAN_POINT('',(11.2,6.2,9.55));
#22585=CARTESIAN_POINT('Origin',(11.2,6.2,9.9));
#22586=CARTESIAN_POINT('',(11.2,7.6,9.68431457505076));
#22587=CARTESIAN_POINT('',(11.2,-6.5,9.68431457505076));
#22588=CARTESIAN_POINT('',(11.2,7.6,9.9));
#22589=CARTESIAN_POINT('',(11.2,6.2,9.9));
#22590=CARTESIAN_POINT('',(11.2,7.6,9.55));
#22591=CARTESIAN_POINT('Origin',(10.8,6.2,9.9));
#22592=CARTESIAN_POINT('',(11.2,7.6,9.9));
#22593=CARTESIAN_POINT('Origin',(11.,7.6,9.725));
#22594=CARTESIAN_POINT('Origin',(11.,7.6,10.25));
#22595=CARTESIAN_POINT('Origin',(11.,6.4,10.25));
#22596=CARTESIAN_POINT('',(10.835,6.4,10.25));
#22597=CARTESIAN_POINT('Origin',(11.,6.4,10.25));
#22598=CARTESIAN_POINT('',(10.835,7.9,10.25));
#22599=CARTESIAN_POINT('',(10.835,6.4,10.25));
#22600=CARTESIAN_POINT('Origin',(11.,7.9,10.25));
#22601=CARTESIAN_POINT('Origin',(11.,6.4,10.25));
#22602=CARTESIAN_POINT('Origin',(11.,-6.6,10.25));
#22603=CARTESIAN_POINT('',(10.835,-6.5,10.25));
#22604=CARTESIAN_POINT('Origin',(11.,-6.5,10.25));
#22605=CARTESIAN_POINT('',(10.835,-4.9,10.25));
#22606=CARTESIAN_POINT('',(10.835,-6.6,10.25));
#22607=CARTESIAN_POINT('Origin',(11.,-4.9,10.25));
#22608=CARTESIAN_POINT('Origin',(11.,-4.9,10.25));
#22609=CARTESIAN_POINT('Origin',(10.8,-0.2,9.55));
#22610=CARTESIAN_POINT('',(10.8,1.2,9.68431457505076));
#22611=CARTESIAN_POINT('',(10.8,-0.2,9.68431457505076));
#22612=CARTESIAN_POINT('',(10.8,-6.5,9.68431457505076));
#22613=CARTESIAN_POINT('',(10.8,1.2,9.9));
#22614=CARTESIAN_POINT('',(10.8,1.2,9.9));
#22615=CARTESIAN_POINT('',(10.8,-0.2,9.9));
#22616=CARTESIAN_POINT('',(10.8,-0.2,9.9));
#22617=CARTESIAN_POINT('',(10.8,-0.2,9.9));
#22618=CARTESIAN_POINT('Origin',(11.,-0.2,9.725));
#22619=CARTESIAN_POINT('',(11.2,-0.2,9.68431457505076));
#22620=CARTESIAN_POINT('Origin',(11.,-0.2,10.25));
#22621=CARTESIAN_POINT('',(11.2,-0.2,9.9));
#22622=CARTESIAN_POINT('',(11.2,-0.2,9.9));
#22623=CARTESIAN_POINT('',(11.2,-0.2,9.55));
#22624=CARTESIAN_POINT('Origin',(11.2,-0.2,9.9));
#22625=CARTESIAN_POINT('',(11.2,1.2,9.68431457505076));
#22626=CARTESIAN_POINT('',(11.2,-6.5,9.68431457505076));
#22627=CARTESIAN_POINT('',(11.2,1.2,9.9));
#22628=CARTESIAN_POINT('',(11.2,-0.2,9.9));
#22629=CARTESIAN_POINT('',(11.2,1.2,9.55));
#22630=CARTESIAN_POINT('Origin',(10.8,-0.2,9.9));
#22631=CARTESIAN_POINT('',(11.2,1.2,9.9));
#22632=CARTESIAN_POINT('Origin',(11.,1.2,9.725));
#22633=CARTESIAN_POINT('Origin',(11.,1.2,10.25));
#22634=CARTESIAN_POINT('Origin',(11.,-1.,10.25));
#22635=CARTESIAN_POINT('',(10.2,-1.,10.25));
#22636=CARTESIAN_POINT('Origin',(11.,-1.,10.25));
#22637=CARTESIAN_POINT('',(10.4,-1.,10.25));
#22638=CARTESIAN_POINT('Origin',(11.,-1.,10.25));
#22639=CARTESIAN_POINT('Origin',(11.,-3.7,10.25));
#22640=CARTESIAN_POINT('',(10.2,-3.7,10.25));
#22641=CARTESIAN_POINT('Origin',(11.,-3.7,10.25));
#22642=CARTESIAN_POINT('',(10.4,-3.7,10.25));
#22643=CARTESIAN_POINT('Origin',(11.,-3.7,10.25));
#22644=CARTESIAN_POINT('Origin',(11.,-3.7,10.25));
#22645=CARTESIAN_POINT('',(10.2,-3.7,10.25));
#22646=CARTESIAN_POINT('Origin',(11.,-6.5,10.25));
#22647=CARTESIAN_POINT('',(10.4,-6.5,10.25));
#22648=CARTESIAN_POINT('',(10.4,-6.5,10.25));
#22649=CARTESIAN_POINT('Origin',(11.,-6.5,10.25));
#22650=CARTESIAN_POINT('Origin',(11.,-6.5,10.25));
#22651=CARTESIAN_POINT('',(10.4,7.9,10.25));
#22652=CARTESIAN_POINT('Origin',(11.,7.9,10.25));
#22653=CARTESIAN_POINT('',(10.4,-6.5,10.25));
#22654=CARTESIAN_POINT('Origin',(11.,7.9,10.25));
#22655=CARTESIAN_POINT('Origin',(11.,-6.5,10.25));
#22656=CARTESIAN_POINT('',(0.,0.,0.));
#22657=CARTESIAN_POINT('Origin',(11.,2.2,10.25));
#22658=CARTESIAN_POINT('',(10.395,3.7,10.25));
#22659=CARTESIAN_POINT('Origin',(11.,3.7,10.25));
#22660=CARTESIAN_POINT('',(10.395,2.2,10.25));
#22661=CARTESIAN_POINT('',(10.395,2.2,10.25));
#22662=CARTESIAN_POINT('Origin',(11.,2.2,10.25));
#22663=CARTESIAN_POINT('Origin',(11.,2.2,10.25));
#22664=CARTESIAN_POINT('',(10.2,3.7,10.25));
#22665=CARTESIAN_POINT('Origin',(11.,3.7,10.25));
#22666=CARTESIAN_POINT('',(10.2,2.2,10.25));
#22667=CARTESIAN_POINT('',(10.2,2.2,10.25));
#22668=CARTESIAN_POINT('Origin',(11.,2.2,10.25));
#22669=CARTESIAN_POINT('Origin',(11.,3.7,10.25));
#22670=CARTESIAN_POINT('Origin',(11.,2.2,10.25));
#22671=CARTESIAN_POINT('',(0.,0.,0.));
#22672=CARTESIAN_POINT('Origin',(11.,-6.,10.25));
#22673=CARTESIAN_POINT('',(10.395,-4.7,10.25));
#22674=CARTESIAN_POINT('Origin',(11.,-4.7,10.25));
#22675=CARTESIAN_POINT('',(10.395,-6.,10.25));
#22676=CARTESIAN_POINT('',(10.395,-6.,10.25));
#22677=CARTESIAN_POINT('Origin',(11.,-6.,10.25));
#22678=CARTESIAN_POINT('Origin',(11.,-6.,10.25));
#22679=CARTESIAN_POINT('',(10.2,-4.7,10.25));
#22680=CARTESIAN_POINT('Origin',(11.,-4.7,10.25));
#22681=CARTESIAN_POINT('',(10.2,-6.,10.25));
#22682=CARTESIAN_POINT('',(10.2,-6.,10.25));
#22683=CARTESIAN_POINT('Origin',(11.,-6.,10.25));
#22684=CARTESIAN_POINT('Origin',(11.,-4.7,10.25));
#22685=CARTESIAN_POINT('Origin',(11.,-6.,10.25));
#22686=CARTESIAN_POINT('',(0.,0.,0.));
#22687=CARTESIAN_POINT('Origin',(11.,4.7,10.25));
#22688=CARTESIAN_POINT('',(10.395,6.,10.25));
#22689=CARTESIAN_POINT('Origin',(11.,6.,10.25));
#22690=CARTESIAN_POINT('',(10.395,4.7,10.25));
#22691=CARTESIAN_POINT('',(10.395,4.7,10.25));
#22692=CARTESIAN_POINT('Origin',(11.,4.7,10.25));
#22693=CARTESIAN_POINT('Origin',(11.,4.7,10.25));
#22694=CARTESIAN_POINT('',(10.2,6.,10.25));
#22695=CARTESIAN_POINT('Origin',(11.,6.,10.25));
#22696=CARTESIAN_POINT('',(10.2,4.7,10.25));
#22697=CARTESIAN_POINT('',(10.2,4.7,10.25));
#22698=CARTESIAN_POINT('Origin',(11.,4.7,10.25));
#22699=CARTESIAN_POINT('Origin',(11.,6.,10.25));
#22700=CARTESIAN_POINT('Origin',(11.,4.7,10.25));
#22701=CARTESIAN_POINT('',(0.,0.,0.));
#22702=CARTESIAN_POINT('Origin',(11.,-6.7,10.25));
#22703=CARTESIAN_POINT('',(10.775,-6.5,10.25));
#22704=CARTESIAN_POINT('Origin',(11.,-6.5,10.25));
#22705=CARTESIAN_POINT('',(10.775,-6.7,10.25));
#22706=CARTESIAN_POINT('',(10.775,-6.7,10.25));
#22707=CARTESIAN_POINT('Origin',(11.,-6.7,10.25));
#22708=CARTESIAN_POINT('Origin',(11.,-6.7,10.25));
#22709=CARTESIAN_POINT('',(10.,-6.5,10.25));
#22710=CARTESIAN_POINT('Origin',(11.,-6.5,10.25));
#22711=CARTESIAN_POINT('',(10.,-6.7,10.25));
#22712=CARTESIAN_POINT('',(10.,-6.7,10.25));
#22713=CARTESIAN_POINT('Origin',(11.,-6.7,10.25));
#22714=CARTESIAN_POINT('Origin',(11.,-6.5,10.25));
#22715=CARTESIAN_POINT('Origin',(11.,-6.7,10.25));
#22716=CARTESIAN_POINT('',(0.,0.,0.));
#22717=CARTESIAN_POINT('Origin',(11.,7.9,10.25));
#22718=CARTESIAN_POINT('',(10.775,8.1,10.25));
#22719=CARTESIAN_POINT('Origin',(11.,8.1,10.25));
#22720=CARTESIAN_POINT('',(10.775,7.9,10.25));
#22721=CARTESIAN_POINT('',(10.775,7.9,10.25));
#22722=CARTESIAN_POINT('Origin',(11.,7.9,10.25));
#22723=CARTESIAN_POINT('Origin',(11.,7.9,10.25));
#22724=CARTESIAN_POINT('',(10.,8.1,10.25));
#22725=CARTESIAN_POINT('Origin',(11.,8.1,10.25));
#22726=CARTESIAN_POINT('',(10.,7.9,10.25));
#22727=CARTESIAN_POINT('',(10.,7.9,10.25));
#22728=CARTESIAN_POINT('Origin',(11.,7.9,10.25));
#22729=CARTESIAN_POINT('Origin',(11.,8.1,10.25));
#22730=CARTESIAN_POINT('Origin',(11.,7.9,10.25));
#22731=CARTESIAN_POINT('',(0.,0.,0.));
#22732=CARTESIAN_POINT('Origin',(11.,-6.5,10.25));
#22733=CARTESIAN_POINT('',(10.395,-6.,10.25));
#22734=CARTESIAN_POINT('Origin',(11.,-6.,10.25));
#22735=CARTESIAN_POINT('',(10.395,-6.5,10.25));
#22736=CARTESIAN_POINT('',(10.395,-6.5,10.25));
#22737=CARTESIAN_POINT('Origin',(11.,-6.5,10.25));
#22738=CARTESIAN_POINT('Origin',(11.,-6.5,10.25));
#22739=CARTESIAN_POINT('',(10.2,-6.,10.25));
#22740=CARTESIAN_POINT('Origin',(11.,-6.,10.25));
#22741=CARTESIAN_POINT('',(10.2,-6.5,10.25));
#22742=CARTESIAN_POINT('',(10.2,-6.5,10.25));
#22743=CARTESIAN_POINT('Origin',(11.,-6.5,10.25));
#22744=CARTESIAN_POINT('Origin',(11.,-6.,10.25));
#22745=CARTESIAN_POINT('Origin',(11.,-6.5,10.25));
#22746=CARTESIAN_POINT('',(0.,0.,0.));
#22747=CARTESIAN_POINT('Origin',(11.,6.4,13.25));
#22748=CARTESIAN_POINT('',(10.75,6.5,13.25));
#22749=CARTESIAN_POINT('Origin',(11.,6.5,13.25));
#22750=CARTESIAN_POINT('',(10.75,7.3,13.25));
#22751=CARTESIAN_POINT('',(10.75,6.4,13.25));
#22752=CARTESIAN_POINT('Origin',(11.,7.3,13.25));
#22753=CARTESIAN_POINT('Origin',(10.8,5.9,9.47));
#22754=CARTESIAN_POINT('',(10.8,6.,9.47));
#22755=CARTESIAN_POINT('',(10.8,6.,9.68431457505076));
#22756=CARTESIAN_POINT('',(10.8,6.,9.86));
#22757=CARTESIAN_POINT('',(10.8,7.9,9.47));
#22758=CARTESIAN_POINT('',(10.8,5.9,9.47));
#22759=CARTESIAN_POINT('',(10.8,7.9,9.68431457505076));
#22760=CARTESIAN_POINT('',(10.8,7.9,9.86));
#22761=CARTESIAN_POINT('',(10.8,6.,9.68431457505076));
#22762=CARTESIAN_POINT('Origin',(11.2,5.9,9.47));
#22763=CARTESIAN_POINT('',(11.2,6.,9.47));
#22764=CARTESIAN_POINT('',(11.1,6.,9.47));
#22765=CARTESIAN_POINT('',(11.2,7.9,9.47));
#22766=CARTESIAN_POINT('',(11.2,5.9,9.47));
#22767=CARTESIAN_POINT('',(11.1,7.9,9.47));
#22768=CARTESIAN_POINT('Origin',(11.2,5.9,10.25));
#22769=CARTESIAN_POINT('',(11.2,6.,9.68431457505076));
#22770=CARTESIAN_POINT('',(11.2,6.,10.25));
#22771=CARTESIAN_POINT('',(11.2,7.9,9.68431457505076));
#22772=CARTESIAN_POINT('',(11.2,6.,9.68431457505076));
#22773=CARTESIAN_POINT('',(11.2,7.9,10.25));
#22774=CARTESIAN_POINT('Origin',(11.,7.9,10.25));
#22775=CARTESIAN_POINT('',(9.8,7.9,10.25));
#22776=CARTESIAN_POINT('Origin',(11.,7.9,10.25));
#22777=CARTESIAN_POINT('Origin',(11.,7.9,10.25));
#22778=CARTESIAN_POINT('Origin',(11.,6.,10.25));
#22779=CARTESIAN_POINT('Origin',(11.,6.,10.25));
#22780=CARTESIAN_POINT('Origin',(11.,6.5,13.25));
#22781=CARTESIAN_POINT('',(11.5,7.3,12.5016685226452));
#22782=CARTESIAN_POINT('',(11.5,6.5,12.5016685226452));
#22783=CARTESIAN_POINT('',(11.5,6.5,12.5016685226452));
#22784=CARTESIAN_POINT('',(10.5,7.3,12.5016685226452));
#22785=CARTESIAN_POINT('Origin',(11.,7.3,13.25));
#22786=CARTESIAN_POINT('',(10.5,6.5,12.5016685226452));
#22787=CARTESIAN_POINT('',(10.5,6.5,12.5016685226452));
#22788=CARTESIAN_POINT('Origin',(11.,6.5,13.25));
#22789=CARTESIAN_POINT('Origin',(11.5,6.5,13.25));
#22790=CARTESIAN_POINT('',(11.5,6.5,11.3408712114636));
#22791=CARTESIAN_POINT('',(11.5,6.5,10.25));
#22792=CARTESIAN_POINT('',(11.5,7.3,11.3408712114636));
#22793=CARTESIAN_POINT('',(11.5,6.,11.3408712114636));
#22794=CARTESIAN_POINT('',(11.5,7.3,10.25));
#22795=CARTESIAN_POINT('Origin',(11.,6.5,11.75));
#22796=CARTESIAN_POINT('',(10.5,6.5,11.3408712114636));
#22797=CARTESIAN_POINT('',(10.5,6.5,13.25));
#22798=CARTESIAN_POINT('Origin',(11.,6.5,10.25));
#22799=CARTESIAN_POINT('Origin',(10.5,6.5,10.25));
#22800=CARTESIAN_POINT('',(10.5,7.3,11.3408712114636));
#22801=CARTESIAN_POINT('',(10.5,7.3,13.25));
#22802=CARTESIAN_POINT('',(10.5,6.,11.3408712114636));
#22803=CARTESIAN_POINT('Origin',(11.,7.3,11.75));
#22804=CARTESIAN_POINT('Origin',(11.,7.3,10.25));
#22805=CARTESIAN_POINT('Origin',(11.,6.,10.25));
#22806=CARTESIAN_POINT('',(9.8,6.,10.25));
#22807=CARTESIAN_POINT('',(9.8,6.,10.25));
#22808=CARTESIAN_POINT('Origin',(11.,6.,10.25));
#22809=CARTESIAN_POINT('Origin',(11.,6.,10.25));
#22810=CARTESIAN_POINT('',(0.,0.,0.));
#22811=CARTESIAN_POINT('Origin',(11.,7.3,13.25));
#22812=CARTESIAN_POINT('',(10.67,8.9,13.25));
#22813=CARTESIAN_POINT('Origin',(11.,8.9,13.25));
#22814=CARTESIAN_POINT('',(10.67,7.3,13.25));
#22815=CARTESIAN_POINT('',(10.67,7.3,13.25));
#22816=CARTESIAN_POINT('Origin',(11.,7.3,13.25));
#22817=CARTESIAN_POINT('Origin',(11.,7.3,13.25));
#22818=CARTESIAN_POINT('',(10.6,8.9,13.25));
#22819=CARTESIAN_POINT('Origin',(11.,8.9,13.25));
#22820=CARTESIAN_POINT('',(10.6,7.3,13.25));
#22821=CARTESIAN_POINT('',(10.6,7.3,13.25));
#22822=CARTESIAN_POINT('Origin',(11.,7.3,13.25));
#22823=CARTESIAN_POINT('Origin',(11.,8.9,13.25));
#22824=CARTESIAN_POINT('Origin',(11.,7.3,13.25));
#22825=CARTESIAN_POINT('',(0.,0.,0.));
#22826=CARTESIAN_POINT('Origin',(0.2,0.,0.));
#22827=CARTESIAN_POINT('',(0.2,2.2,-0.78));
#22828=CARTESIAN_POINT('',(0.2,2.2,-0.565685424949238));
#22829=CARTESIAN_POINT('',(0.2,2.2,0.));
#22830=CARTESIAN_POINT('',(0.2,-1.,-0.78));
#22831=CARTESIAN_POINT('',(0.2,0.,-0.78));
#22832=CARTESIAN_POINT('',(0.2,-1.,-0.565685424949238));
#22833=CARTESIAN_POINT('',(0.2,-1.,0.));
#22834=CARTESIAN_POINT('',(0.2,0.,-0.565685424949238));
#22835=CARTESIAN_POINT('Origin',(0.2,0.,-0.78));
#22836=CARTESIAN_POINT('',(-0.2,2.2,-0.78));
#22837=CARTESIAN_POINT('',(0.1,2.2,-0.78));
#22838=CARTESIAN_POINT('',(-0.2,-1.,-0.78));
#22839=CARTESIAN_POINT('',(-0.2,0.,-0.78));
#22840=CARTESIAN_POINT('',(0.1,-1.,-0.78));
#22841=CARTESIAN_POINT('Origin',(-0.2,0.,-0.78));
#22842=CARTESIAN_POINT('',(-0.2,2.2,-0.565685424949238));
#22843=CARTESIAN_POINT('',(-0.2,2.2,-0.39));
#22844=CARTESIAN_POINT('',(-0.2,-1.,-0.565685424949238));
#22845=CARTESIAN_POINT('',(-0.2,0.,-0.565685424949238));
#22846=CARTESIAN_POINT('',(-0.2,-1.,-0.39));
#22847=CARTESIAN_POINT('Origin',(0.,-1.,0.));
#22848=CARTESIAN_POINT('',(1.60662857109684,-1.,0.693717979106306));
#22849=CARTESIAN_POINT('',(1.5055822144029,-1.,0.892032620296856));
#22850=CARTESIAN_POINT('Origin',(0.,-1.,0.));
#22851=CARTESIAN_POINT('',(1.81978687191668,-1.,1.23627494547115));
#22852=CARTESIAN_POINT('Ctrl Pts',(1.5055822144029,-1.,0.892032620296856));
#22853=CARTESIAN_POINT('Ctrl Pts',(1.50980486806688,-1.,0.894452006964544));
#22854=CARTESIAN_POINT('Ctrl Pts',(1.51805569590094,-1.,0.899185047483511));
#22855=CARTESIAN_POINT('Ctrl Pts',(1.52984849887993,-1.,0.905967409625651));
#22856=CARTESIAN_POINT('Ctrl Pts',(1.54440491149498,-1.,0.914375919026456));
#22857=CARTESIAN_POINT('Ctrl Pts',(1.56065988578893,-1.,0.923832188944341));
#22858=CARTESIAN_POINT('Ctrl Pts',(1.57499388382243,-1.,0.932246680108685));
#22859=CARTESIAN_POINT('Ctrl Pts',(1.58744937487176,-1.,0.939646377893399));
#22860=CARTESIAN_POINT('Ctrl Pts',(1.59810042043673,-1.,0.946078063315257));
#22861=CARTESIAN_POINT('Ctrl Pts',(1.60706069896936,-1.,0.951613284356035));
#22862=CARTESIAN_POINT('Ctrl Pts',(1.61449324337085,-1.,0.956354422920671));
#22863=CARTESIAN_POINT('Ctrl Pts',(1.62061638140221,-1.,0.960438326101729));
#22864=CARTESIAN_POINT('Ctrl Pts',(1.62571930670187,-1.,0.964046107040536));
#22865=CARTESIAN_POINT('Ctrl Pts',(1.63013849959461,-1.,0.967387853230345));
#22866=CARTESIAN_POINT('Ctrl Pts',(1.63420665729798,-1.,0.970669715997509));
#22867=CARTESIAN_POINT('Ctrl Pts',(1.63820952658144,-1.,0.974066058287419));
#22868=CARTESIAN_POINT('Ctrl Pts',(1.64233990826687,-1.,0.977689794119417));
#22869=CARTESIAN_POINT('Ctrl Pts',(1.64665139190656,-1.,0.981562530939489));
#22870=CARTESIAN_POINT('Ctrl Pts',(1.65110016612638,-1.,0.985642622920821));
#22871=CARTESIAN_POINT('Ctrl Pts',(1.65559044289699,-1.,0.989855627854165));
#22872=CARTESIAN_POINT('Ctrl Pts',(1.66001553809947,-1.,0.994121836661306));
#22873=CARTESIAN_POINT('Ctrl Pts',(1.66430758030376,-1.,0.998389654952758));
#22874=CARTESIAN_POINT('Ctrl Pts',(1.66846059277303,-1.,1.00265091003727));
#22875=CARTESIAN_POINT('Ctrl Pts',(1.67250335383293,-1.,1.00692206696414));
#22876=CARTESIAN_POINT('Ctrl Pts',(1.67648246776464,-1.,1.01123236493511));
#22877=CARTESIAN_POINT('Ctrl Pts',(1.68044289894798,-1.,1.01561026162773));
#22878=CARTESIAN_POINT('Ctrl Pts',(1.68440578021706,-1.,1.02006795074201));
#22879=CARTESIAN_POINT('Ctrl Pts',(1.68836910178447,-1.,1.02460180535255));
#22880=CARTESIAN_POINT('Ctrl Pts',(1.69231840863458,-1.,1.02919977579147));
#22881=CARTESIAN_POINT('Ctrl Pts',(1.69623414782771,-1.,1.03384646003588));
#22882=CARTESIAN_POINT('Ctrl Pts',(1.70010052930962,-1.,1.03852922490789));
#22883=CARTESIAN_POINT('Ctrl Pts',(1.70391338707982,-1.,1.04324363334554));
#22884=CARTESIAN_POINT('Ctrl Pts',(1.70767646263649,-1.,1.04799085404995));
#22885=CARTESIAN_POINT('Ctrl Pts',(1.71139783543989,-1.,1.05277517202855));
#22886=CARTESIAN_POINT('Ctrl Pts',(1.7150865442702,-1.,1.05760163192479));
#22887=CARTESIAN_POINT('Ctrl Pts',(1.71874858456904,-1.,1.06247324680647));
#22888=CARTESIAN_POINT('Ctrl Pts',(1.72238500928453,-1.,1.06738966975462));
#22889=CARTESIAN_POINT('Ctrl Pts',(1.72599406198488,-1.,1.07234866990252));
#22890=CARTESIAN_POINT('Ctrl Pts',(1.72957248977424,-1.,1.0773470373727));
#22891=CARTESIAN_POINT('Ctrl Pts',(1.73311705663407,-1.,1.08238162784749));
#22892=CARTESIAN_POINT('Ctrl Pts',(1.73662628326091,-1.,1.08745056285427));
#22893=CARTESIAN_POINT('Ctrl Pts',(1.74010053962247,-1.,1.09255329056493));
#22894=CARTESIAN_POINT('Ctrl Pts',(1.74354119236208,-1.,1.09768999241226));
#22895=CARTESIAN_POINT('Ctrl Pts',(1.74695004214923,-1.,1.10286118991143));
#22896=CARTESIAN_POINT('Ctrl Pts',(1.7503286607592,-1.,1.10806728183007));
#22897=CARTESIAN_POINT('Ctrl Pts',(1.7536777209463,-1.,1.11330807582551));
#22898=CARTESIAN_POINT('Ctrl Pts',(1.75699720772105,-1.,1.11858293216763));
#22899=CARTESIAN_POINT('Ctrl Pts',(1.76028671825096,-1.,1.12389096855086));
#22900=CARTESIAN_POINT('Ctrl Pts',(1.7635457196617,-1.,1.12923123555075));
#22901=CARTESIAN_POINT('Ctrl Pts',(1.76677384551862,-1.,1.1346029180462));
#22902=CARTESIAN_POINT('Ctrl Pts',(1.76997111386769,-1.,1.14000548336975));
#22903=CARTESIAN_POINT('Ctrl Pts',(1.77313777896194,-1.,1.1454385822692));
#22904=CARTESIAN_POINT('Ctrl Pts',(1.7762742255701,-1.,1.15090197841515));
#22905=CARTESIAN_POINT('Ctrl Pts',(1.77938085564275,-1.,1.15639547194698));
#22906=CARTESIAN_POINT('Ctrl Pts',(1.78245795881009,-1.,1.16191881298499));
#22907=CARTESIAN_POINT('Ctrl Pts',(1.78550566040443,-1.,1.16747166312303));
#22908=CARTESIAN_POINT('Ctrl Pts',(1.78852398877616,-1.,1.17305363177328));
#22909=CARTESIAN_POINT('Ctrl Pts',(1.79151291552689,-1.,1.17866429440809));
#22910=CARTESIAN_POINT('Ctrl Pts',(1.79447240321515,-1.,1.18430321697432));
#22911=CARTESIAN_POINT('Ctrl Pts',(1.79740245923478,-1.,1.18996997934445));
#22912=CARTESIAN_POINT('Ctrl Pts',(1.80030314369879,-1.,1.19566418930242));
#22913=CARTESIAN_POINT('Ctrl Pts',(1.80317454838603,-1.,1.20138548938974));
#22914=CARTESIAN_POINT('Ctrl Pts',(1.80601678480707,-1.,1.20713356605475));
#22915=CARTESIAN_POINT('Ctrl Pts',(1.80882996917129,-1.,1.21290815708314));
#22916=CARTESIAN_POINT('Ctrl Pts',(1.81161420806656,-1.,1.21870906103557));
#22917=CARTESIAN_POINT('Ctrl Pts',(1.81436959210434,-1.,1.2245361330495));
#22918=CARTESIAN_POINT('Ctrl Pts',(1.8165508718364,-1.,1.2292186489137));
#22919=CARTESIAN_POINT('Ctrl Pts',(1.81817389921279,-1.,1.2327422452705));
#22920=CARTESIAN_POINT('Ctrl Pts',(1.81925017193666,-1.,1.23509651170476));
#22921=CARTESIAN_POINT('Ctrl Pts',(1.81978687191668,-1.,1.23627494547115));
#22922=CARTESIAN_POINT('',(1.73811241238545,-1.,1.34869019493419));
#22923=CARTESIAN_POINT('',(1.81978687191668,-1.,1.23627494547115));
#22924=CARTESIAN_POINT('',(1.31362392696032,-1.,1.15624053661742));
#22925=CARTESIAN_POINT('Ctrl Pts',(1.73811241238545,-1.,1.34869019493419));
#22926=CARTESIAN_POINT('Ctrl Pts',(1.73682580585691,-1.,1.34854391898045));
#22927=CARTESIAN_POINT('Ctrl Pts',(1.73425417885907,-1.,1.34824783112887));
#22928=CARTESIAN_POINT('Ctrl Pts',(1.7304014965394,-1.,1.34779309152035));
#22929=CARTESIAN_POINT('Ctrl Pts',(1.72527410680674,-1.,1.34716554819527));
#22930=CARTESIAN_POINT('Ctrl Pts',(1.7188807715049,-1.,1.34634568653227));
#22931=CARTESIAN_POINT('Ctrl Pts',(1.71250340686822,-1.,1.34549029589416));
#22932=CARTESIAN_POINT('Ctrl Pts',(1.70614212266738,-1.,1.34459924533831));
#22933=CARTESIAN_POINT('Ctrl Pts',(1.69979707754427,-1.,1.34367237124483));
#22934=CARTESIAN_POINT('Ctrl Pts',(1.6934684849687,-1.,1.34270948206319));
#22935=CARTESIAN_POINT('Ctrl Pts',(1.68715660868764,-1.,1.341710374848));
#22936=CARTESIAN_POINT('Ctrl Pts',(1.68086176030362,-1.,1.34067485185203));
#22937=CARTESIAN_POINT('Ctrl Pts',(1.67458429426086,-1.,1.3396027347034));
#22938=CARTESIAN_POINT('Ctrl Pts',(1.66832460783989,-1.,1.33849388654388));
#22939=CARTESIAN_POINT('Ctrl Pts',(1.66208312541983,-1.,1.33734820885262));
#22940=CARTESIAN_POINT('Ctrl Pts',(1.65586025952593,-1.,1.33616559745172));
#22941=CARTESIAN_POINT('Ctrl Pts',(1.6496563728683,-1.,1.33494590467993));
#22942=CARTESIAN_POINT('Ctrl Pts',(1.6434717485603,-1.,1.33368890676572));
#22943=CARTESIAN_POINT('Ctrl Pts',(1.63730653475089,-1.,1.33239425103724));
#22944=CARTESIAN_POINT('Ctrl Pts',(1.63116079730923,-1.,1.33106149345645));
#22945=CARTESIAN_POINT('Ctrl Pts',(1.62503464209797,-1.,1.3296901950568));
#22946=CARTESIAN_POINT('Ctrl Pts',(1.61892832270724,-1.,1.32828000610449));
#22947=CARTESIAN_POINT('Ctrl Pts',(1.6128423401575,-1.,1.32683074483356));
#22948=CARTESIAN_POINT('Ctrl Pts',(1.60677758290954,-1.,1.32534250785782));
#22949=CARTESIAN_POINT('Ctrl Pts',(1.60073511858687,-1.,1.32381550858256));
#22950=CARTESIAN_POINT('Ctrl Pts',(1.59471591079403,-1.,1.32224985747682));
#22951=CARTESIAN_POINT('Ctrl Pts',(1.58872057258245,-1.,1.32064537110892));
#22952=CARTESIAN_POINT('Ctrl Pts',(1.58274907898834,-1.,1.31900135021432));
#22953=CARTESIAN_POINT('Ctrl Pts',(1.5768005650559,-1.,1.31731642317187));
#22954=CARTESIAN_POINT('Ctrl Pts',(1.57087397835723,-1.,1.31558903860016));
#22955=CARTESIAN_POINT('Ctrl Pts',(1.56496872402353,-1.,1.31381795281002));
#22956=CARTESIAN_POINT('Ctrl Pts',(1.55908521254821,-1.,1.31200264341696));
#22957=CARTESIAN_POINT('Ctrl Pts',(1.55322568759481,-1.,1.31014393684222));
#22958=CARTESIAN_POINT('Ctrl Pts',(1.54739413957185,-1.,1.30824393907473));
#22959=CARTESIAN_POINT('Ctrl Pts',(1.54159462645432,-1.,1.30630475189556));
#22960=CARTESIAN_POINT('Ctrl Pts',(1.53582981268977,-1.,1.30432735639489));
#22961=CARTESIAN_POINT('Ctrl Pts',(1.53009970283891,-1.,1.30231064395568));
#22962=CARTESIAN_POINT('Ctrl Pts',(1.52439957861062,-1.,1.30024984366328));
#22963=CARTESIAN_POINT('Ctrl Pts',(1.51872184912724,-1.,1.29813791800747));
#22964=CARTESIAN_POINT('Ctrl Pts',(1.51305994241402,-1.,1.29596850710509));
#22965=CARTESIAN_POINT('Ctrl Pts',(1.50741159078365,-1.,1.29373841372842));
#22966=CARTESIAN_POINT('Ctrl Pts',(1.50178230149776,-1.,1.29145022885181));
#22967=CARTESIAN_POINT('Ctrl Pts',(1.49618896881754,-1.,1.28911506584254));
#22968=CARTESIAN_POINT('Ctrl Pts',(1.4906522831278,-1.,1.2867467611644));
#22969=CARTESIAN_POINT('Ctrl Pts',(1.4851881711891,-1.,1.28435533880201));
#22970=CARTESIAN_POINT('Ctrl Pts',(1.47980070347095,-1.,1.28194158939517));
#22971=CARTESIAN_POINT('Ctrl Pts',(1.4744717526707,-1.,1.2794891824849));
#22972=CARTESIAN_POINT('Ctrl Pts',(1.46916035917133,-1.,1.2769641483109));
#22973=CARTESIAN_POINT('Ctrl Pts',(1.46382431332476,-1.,1.27433119897822));
#22974=CARTESIAN_POINT('Ctrl Pts',(1.45843906294697,-1.,1.27156805265289));
#22975=CARTESIAN_POINT('Ctrl Pts',(1.45301422764247,-1.,1.2686778680489));
#22976=CARTESIAN_POINT('Ctrl Pts',(1.44761985001662,-1.,1.26570925118868));
#22977=CARTESIAN_POINT('Ctrl Pts',(1.44236470511303,-1.,1.26273903323859));
#22978=CARTESIAN_POINT('Ctrl Pts',(1.43734919180847,-1.,1.25983531012005));
#22979=CARTESIAN_POINT('Ctrl Pts',(1.43262645609691,-1.,1.25702687965755));
#22980=CARTESIAN_POINT('Ctrl Pts',(1.42815938799387,-1.,1.25426945222639));
#22981=CARTESIAN_POINT('Ctrl Pts',(1.42378102115575,-1.,1.2514145557001));
#22982=CARTESIAN_POINT('Ctrl Pts',(1.41923722596025,-1.,1.24824430986571));
#22983=CARTESIAN_POINT('Ctrl Pts',(1.41422913175179,-1.,1.24450600513056));
#22984=CARTESIAN_POINT('Ctrl Pts',(1.40845295531283,-1.,1.23994455029534));
#22985=CARTESIAN_POINT('Ctrl Pts',(1.40164708206106,-1.,1.23434087290423));
#22986=CARTESIAN_POINT('Ctrl Pts',(1.39361389568796,-1.,1.22752961899387));
#22987=CARTESIAN_POINT('Ctrl Pts',(1.38420564527715,-1.,1.21938737280852));
#22988=CARTESIAN_POINT('Ctrl Pts',(1.37331915607905,-1.,1.20982812925645));
#22989=CARTESIAN_POINT('Ctrl Pts',(1.36088705043885,-1.,1.1987959077932));
#22990=CARTESIAN_POINT('Ctrl Pts',(1.34687054001093,-1.,1.18625865667441));
#22991=CARTESIAN_POINT('Ctrl Pts',(1.33437539347008,-1.,1.17501305789857));
#22992=CARTESIAN_POINT('Ctrl Pts',(1.32428080721772,-1.,1.16589330093588));
#22993=CARTESIAN_POINT('Ctrl Pts',(1.31722977216397,-1.,1.15950888730809));
#22994=CARTESIAN_POINT('Ctrl Pts',(1.31362392696032,-1.,1.15624053661742));
#22995=CARTESIAN_POINT('',(1.15624053661742,-1.,1.31362392696033));
#22996=CARTESIAN_POINT('Origin',(0.,-1.,0.));
#22997=CARTESIAN_POINT('',(1.34869019493419,-1.,1.73811241238545));
#22998=CARTESIAN_POINT('Ctrl Pts',(1.15624053661742,-1.,1.31362392696033));
#22999=CARTESIAN_POINT('Ctrl Pts',(1.15950888730433,-1.,1.3172297721596));
#23000=CARTESIAN_POINT('Ctrl Pts',(1.16589330092532,-1.,1.32428080720544));
#23001=CARTESIAN_POINT('Ctrl Pts',(1.17501305787994,-1.,1.33437539344842));
#23002=CARTESIAN_POINT('Ctrl Pts',(1.18625865664915,-1.,1.34687053998157));
#23003=CARTESIAN_POINT('Ctrl Pts',(1.1987959077656,-1.,1.36088705040677));
#23004=CARTESIAN_POINT('Ctrl Pts',(1.20982812923113,-1.,1.37331915604962));
#23005=CARTESIAN_POINT('Ctrl Pts',(1.21938737278853,-1.,1.38420564525391));
#23006=CARTESIAN_POINT('Ctrl Pts',(1.22752961898063,-1.,1.39361389567257));
#23007=CARTESIAN_POINT('Ctrl Pts',(1.23434087289768,-1.,1.40164708205345));
#23008=CARTESIAN_POINT('Ctrl Pts',(1.23994455029421,-1.,1.40845295531151));
#23009=CARTESIAN_POINT('Ctrl Pts',(1.24450600513278,-1.,1.41422913175437));
#23010=CARTESIAN_POINT('Ctrl Pts',(1.24824430986911,-1.,1.41923722596421));
#23011=CARTESIAN_POINT('Ctrl Pts',(1.25141455570299,-1.,1.42378102115911));
#23012=CARTESIAN_POINT('Ctrl Pts',(1.25426945222783,-1.,1.42815938799555));
#23013=CARTESIAN_POINT('Ctrl Pts',(1.25702687965744,-1.,1.43262645609679));
#23014=CARTESIAN_POINT('Ctrl Pts',(1.25983531011894,-1.,1.43734919180719));
#23015=CARTESIAN_POINT('Ctrl Pts',(1.26273903323723,-1.,1.44236470511145));
#23016=CARTESIAN_POINT('Ctrl Pts',(1.26570925118767,-1.,1.44761985001544));
#23017=CARTESIAN_POINT('Ctrl Pts',(1.26867786804854,-1.,1.45301422764205));
#23018=CARTESIAN_POINT('Ctrl Pts',(1.27156805265312,-1.,1.45843906294725));
#23019=CARTESIAN_POINT('Ctrl Pts',(1.27433119897877,-1.,1.4638243133254));
#23020=CARTESIAN_POINT('Ctrl Pts',(1.27696414831144,-1.,1.46916035917197));
#23021=CARTESIAN_POINT('Ctrl Pts',(1.27948918248524,-1.,1.4744717526711));
#23022=CARTESIAN_POINT('Ctrl Pts',(1.28194158939522,-1.,1.47980070347102));
#23023=CARTESIAN_POINT('Ctrl Pts',(1.28435533880184,-1.,1.48518817118891));
#23024=CARTESIAN_POINT('Ctrl Pts',(1.28674676116415,-1.,1.4906522831275));
#23025=CARTESIAN_POINT('Ctrl Pts',(1.28911506584232,-1.,1.49618896881729));
#23026=CARTESIAN_POINT('Ctrl Pts',(1.29145022885171,-1.,1.50178230149764));
#23027=CARTESIAN_POINT('Ctrl Pts',(1.29373841372843,-1.,1.50741159078367));
#23028=CARTESIAN_POINT('Ctrl Pts',(1.29596850710518,-1.,1.51305994241412));
#23029=CARTESIAN_POINT('Ctrl Pts',(1.29813791800757,-1.,1.51872184912735));
#23030=CARTESIAN_POINT('Ctrl Pts',(1.30024984366334,-1.,1.5243995786107));
#23031=CARTESIAN_POINT('Ctrl Pts',(1.3023106439557,-1.,1.53009970283893));
#23032=CARTESIAN_POINT('Ctrl Pts',(1.30432735639487,-1.,1.53582981268976));
#23033=CARTESIAN_POINT('Ctrl Pts',(1.30630475189553,-1.,1.54159462645428));
#23034=CARTESIAN_POINT('Ctrl Pts',(1.30824393907471,-1.,1.54739413957183));
#23035=CARTESIAN_POINT('Ctrl Pts',(1.31014393684221,-1.,1.55322568759481));
#23036=CARTESIAN_POINT('Ctrl Pts',(1.31200264341696,-1.,1.55908521254822));
#23037=CARTESIAN_POINT('Ctrl Pts',(1.31381795281002,-1.,1.56496872402352));
#23038=CARTESIAN_POINT('Ctrl Pts',(1.31558903860015,-1.,1.57087397835721));
#23039=CARTESIAN_POINT('Ctrl Pts',(1.31731642317183,-1.,1.57680056505585));
#23040=CARTESIAN_POINT('Ctrl Pts',(1.31900135021428,-1.,1.58274907898829));
#23041=CARTESIAN_POINT('Ctrl Pts',(1.32064537110891,-1.,1.58872057258244));
#23042=CARTESIAN_POINT('Ctrl Pts',(1.32224985747686,-1.,1.59471591079408));
#23043=CARTESIAN_POINT('Ctrl Pts',(1.32381550858266,-1.,1.600735118587));
#23044=CARTESIAN_POINT('Ctrl Pts',(1.32534250785794,-1.,1.6067775829097));
#23045=CARTESIAN_POINT('Ctrl Pts',(1.32683074483365,-1.,1.61284234015762));
#23046=CARTESIAN_POINT('Ctrl Pts',(1.32828000610448,-1.,1.61892832270723));
#23047=CARTESIAN_POINT('Ctrl Pts',(1.32969019505665,-1.,1.62503464209777));
#23048=CARTESIAN_POINT('Ctrl Pts',(1.33106149345618,-1.,1.63116079730887));
#23049=CARTESIAN_POINT('Ctrl Pts',(1.33239425103694,-1.,1.6373065347505));
#23050=CARTESIAN_POINT('Ctrl Pts',(1.33368890676554,-1.,1.64347174856007));
#23051=CARTESIAN_POINT('Ctrl Pts',(1.33494590468003,-1.,1.64965637286843));
#23052=CARTESIAN_POINT('Ctrl Pts',(1.33616559745217,-1.,1.65586025952651));
#23053=CARTESIAN_POINT('Ctrl Pts',(1.33734820885331,-1.,1.66208312542073));
#23054=CARTESIAN_POINT('Ctrl Pts',(1.33849388654458,-1.,1.66832460784078));
#23055=CARTESIAN_POINT('Ctrl Pts',(1.33960273470372,-1.,1.67458429426126));
#23056=CARTESIAN_POINT('Ctrl Pts',(1.3406748518516,-1.,1.68086176030308));
#23057=CARTESIAN_POINT('Ctrl Pts',(1.34171037484673,-1.,1.68715660868602));
#23058=CARTESIAN_POINT('Ctrl Pts',(1.34270948206139,-1.,1.6934684849664));
#23059=CARTESIAN_POINT('Ctrl Pts',(1.34367237124322,-1.,1.69979707754221));
#23060=CARTESIAN_POINT('Ctrl Pts',(1.34459924533783,-1.,1.70614212266676));
#23061=CARTESIAN_POINT('Ctrl Pts',(1.34549029589563,-1.,1.71250340687011));
#23062=CARTESIAN_POINT('Ctrl Pts',(1.34634568653586,-1.,1.7188807715095));
#23063=CARTESIAN_POINT('Ctrl Pts',(1.34716554820013,-1.,1.72527410681298));
#23064=CARTESIAN_POINT('Ctrl Pts',(1.3477930915247,-1.,1.73040149654497));
#23065=CARTESIAN_POINT('Ctrl Pts',(1.34824783113158,-1.,1.73425417886255));
#23066=CARTESIAN_POINT('Ctrl Pts',(1.34854391898145,-1.,1.73682580585819));
#23067=CARTESIAN_POINT('Ctrl Pts',(1.34869019493419,-1.,1.73811241238545));
#23068=CARTESIAN_POINT('',(1.23627494547115,-1.,1.81978687191668));
#23069=CARTESIAN_POINT('',(1.34869019493419,-1.,1.73811241238545));
#23070=CARTESIAN_POINT('',(0.892032620296855,-1.,1.5055822144029));
#23071=CARTESIAN_POINT('Ctrl Pts',(1.23627494547115,-1.,1.81978687191668));
#23072=CARTESIAN_POINT('Ctrl Pts',(1.23509651170384,-1.,1.81925017193531));
#23073=CARTESIAN_POINT('Ctrl Pts',(1.23274224526804,-1.,1.81817389920914));
#23074=CARTESIAN_POINT('Ctrl Pts',(1.22921864890975,-1.,1.81655087183054));
#23075=CARTESIAN_POINT('Ctrl Pts',(1.22453613304507,-1.,1.81436959209778));
#23076=CARTESIAN_POINT('Ctrl Pts',(1.2187090610323,-1.,1.81161420806172));
#23077=CARTESIAN_POINT('Ctrl Pts',(1.2129081570818,-1.,1.80882996916931));
#23078=CARTESIAN_POINT('Ctrl Pts',(1.20713356605519,-1.,1.80601678480772));
#23079=CARTESIAN_POINT('Ctrl Pts',(1.2013854893912,-1.,1.8031745483882));
#23080=CARTESIAN_POINT('Ctrl Pts',(1.19566418930405,-1.,1.80030314370121));
#23081=CARTESIAN_POINT('Ctrl Pts',(1.1899699793456,-1.,1.79740245923649));
#23082=CARTESIAN_POINT('Ctrl Pts',(1.18430321697471,-1.,1.79447240321572));
#23083=CARTESIAN_POINT('Ctrl Pts',(1.17866429440781,-1.,1.79151291552646));
#23084=CARTESIAN_POINT('Ctrl Pts',(1.17305363177265,-1.,1.78852398877523));
#23085=CARTESIAN_POINT('Ctrl Pts',(1.16747166312239,-1.,1.78550566040349));
#23086=CARTESIAN_POINT('Ctrl Pts',(1.16191881298458,-1.,1.78245795880949));
#23087=CARTESIAN_POINT('Ctrl Pts',(1.15639547194689,-1.,1.77938085564261));
#23088=CARTESIAN_POINT('Ctrl Pts',(1.15090197841531,-1.,1.77627422557034));
#23089=CARTESIAN_POINT('Ctrl Pts',(1.14543858226948,-1.,1.77313777896234));
#23090=CARTESIAN_POINT('Ctrl Pts',(1.14000548337,-1.,1.76997111386806));
#23091=CARTESIAN_POINT('Ctrl Pts',(1.13460291804634,-1.,1.76677384551883));
#23092=CARTESIAN_POINT('Ctrl Pts',(1.12923123555076,-1.,1.76354571966171));
#23093=CARTESIAN_POINT('Ctrl Pts',(1.12389096855078,-1.,1.76028671825084));
#23094=CARTESIAN_POINT('Ctrl Pts',(1.11858293216752,-1.,1.75699720772089));
#23095=CARTESIAN_POINT('Ctrl Pts',(1.11330807582542,-1.,1.75367772094617));
#23096=CARTESIAN_POINT('Ctrl Pts',(1.10806728183003,-1.,1.75032866075914));
#23097=CARTESIAN_POINT('Ctrl Pts',(1.10286118991144,-1.,1.74695004214924));
#23098=CARTESIAN_POINT('Ctrl Pts',(1.09768999241229,-1.,1.74354119236212));
#23099=CARTESIAN_POINT('Ctrl Pts',(1.09255329056496,-1.,1.74010053962252));
#23100=CARTESIAN_POINT('Ctrl Pts',(1.08745056285429,-1.,1.73662628326093));
#23101=CARTESIAN_POINT('Ctrl Pts',(1.08238162784749,-1.,1.73311705663407));
#23102=CARTESIAN_POINT('Ctrl Pts',(1.0773470373727,-1.,1.72957248977424));
#23103=CARTESIAN_POINT('Ctrl Pts',(1.07234866990252,-1.,1.72599406198489));
#23104=CARTESIAN_POINT('Ctrl Pts',(1.06738966975463,-1.,1.72238500928456));
#23105=CARTESIAN_POINT('Ctrl Pts',(1.06247324680649,-1.,1.71874858456908));
#23106=CARTESIAN_POINT('Ctrl Pts',(1.05760163192481,-1.,1.71508654427022));
#23107=CARTESIAN_POINT('Ctrl Pts',(1.05277517202853,-1.,1.71139783543986));
#23108=CARTESIAN_POINT('Ctrl Pts',(1.0479908540499,-1.,1.70767646263641));
#23109=CARTESIAN_POINT('Ctrl Pts',(1.04324363334546,-1.,1.70391338707969));
#23110=CARTESIAN_POINT('Ctrl Pts',(1.03852922490782,-1.,1.70010052930951));
#23111=CARTESIAN_POINT('Ctrl Pts',(1.03384646003587,-1.,1.69623414782769));
#23112=CARTESIAN_POINT('Ctrl Pts',(1.02919977579155,-1.,1.69231840863471));
#23113=CARTESIAN_POINT('Ctrl Pts',(1.02460180535272,-1.,1.68836910178475));
#23114=CARTESIAN_POINT('Ctrl Pts',(1.02006795074222,-1.,1.68440578021739));
#23115=CARTESIAN_POINT('Ctrl Pts',(1.01561026162786,-1.,1.6804428989482));
#23116=CARTESIAN_POINT('Ctrl Pts',(1.01123236493507,-1.,1.67648246776457));
#23117=CARTESIAN_POINT('Ctrl Pts',(1.00692206696387,-1.,1.67250335383248));
#23118=CARTESIAN_POINT('Ctrl Pts',(1.00265091003682,-1.,1.66846059277231));
#23119=CARTESIAN_POINT('Ctrl Pts',(0.998389654952317,-1.,1.66430758030304));
#23120=CARTESIAN_POINT('Ctrl Pts',(0.994121836661115,-1.,1.66001553809916));
#23121=CARTESIAN_POINT('Ctrl Pts',(0.98985562785445,-1.,1.65559044289746));
#23122=CARTESIAN_POINT('Ctrl Pts',(0.985642622921626,-1.,1.6511001661277));
#23123=CARTESIAN_POINT('Ctrl Pts',(0.981562530940574,-1.,1.64665139190834));
#23124=CARTESIAN_POINT('Ctrl Pts',(0.977689794120296,-1.,1.64233990826831));
#23125=CARTESIAN_POINT('Ctrl Pts',(0.974066058287501,-1.,1.63820952658157));
#23126=CARTESIAN_POINT('Ctrl Pts',(0.970669715996356,-1.,1.63420665729609));
#23127=CARTESIAN_POINT('Ctrl Pts',(0.967387853228041,-1.,1.63013849959083));
#23128=CARTESIAN_POINT('Ctrl Pts',(0.964046107037821,-1.,1.6257193066974));
#23129=CARTESIAN_POINT('Ctrl Pts',(0.960438326099958,-1.,1.62061638139929));
#23130=CARTESIAN_POINT('Ctrl Pts',(0.956354422921572,-1.,1.61449324337233));
#23131=CARTESIAN_POINT('Ctrl Pts',(0.951613284361247,-1.,1.60706069897794));
#23132=CARTESIAN_POINT('Ctrl Pts',(0.946078063325795,-1.,1.59810042045408));
#23133=CARTESIAN_POINT('Ctrl Pts',(0.939646377909319,-1.,1.58744937489796));
#23134=CARTESIAN_POINT('Ctrl Pts',(0.932246680128848,-1.,1.57499388385561));
#23135=CARTESIAN_POINT('Ctrl Pts',(0.923832188966322,-1.,1.56065988582509));
#23136=CARTESIAN_POINT('Ctrl Pts',(0.914375919046579,-1.,1.54440491152808));
#23137=CARTESIAN_POINT('Ctrl Pts',(0.905967409640498,-1.,1.52984849890434));
#23138=CARTESIAN_POINT('Ctrl Pts',(0.89918504749193,-1.,1.51805569591479));
#23139=CARTESIAN_POINT('Ctrl Pts',(0.894452006967538,-1.,1.50980486807181));
#23140=CARTESIAN_POINT('Ctrl Pts',(0.892032620296855,-1.,1.5055822144029));
#23141=CARTESIAN_POINT('',(0.693717979106305,-1.,1.60662857109684));
#23142=CARTESIAN_POINT('Origin',(0.,-1.,0.));
#23143=CARTESIAN_POINT('',(0.7455743247944,-1.,2.0698113262342));
#23144=CARTESIAN_POINT('Ctrl Pts',(0.693717979106305,-1.,1.60662857109684));
#23145=CARTESIAN_POINT('Ctrl Pts',(0.69571209787897,-1.,1.61106790957619));
#23146=CARTESIAN_POINT('Ctrl Pts',(0.699605146398836,-1.,1.61974673471117));
#23147=CARTESIAN_POINT('Ctrl Pts',(0.705159151977294,-1.,1.6321654166204));
#23148=CARTESIAN_POINT('Ctrl Pts',(0.711993139340447,-1.,1.64752408828442));
#23149=CARTESIAN_POINT('Ctrl Pts',(0.719585433787949,-1.,1.66472880551777));
#23150=CARTESIAN_POINT('Ctrl Pts',(0.726235967982445,-1.,1.67996158451922));
#23151=CARTESIAN_POINT('Ctrl Pts',(0.731963238685357,-1.,1.69326921972915));
#23152=CARTESIAN_POINT('Ctrl Pts',(0.736799665716932,-1.,1.70473309004249));
#23153=CARTESIAN_POINT('Ctrl Pts',(0.74079516202821,-1.,1.71447789751001));
#23154=CARTESIAN_POINT('Ctrl Pts',(0.744021445433093,-1.,1.72268229916769));
#23155=CARTESIAN_POINT('Ctrl Pts',(0.746574710097752,-1.,1.72958533647714));
#23156=CARTESIAN_POINT('Ctrl Pts',(0.74858246295687,-1.,1.7355035168033));
#23157=CARTESIAN_POINT('Ctrl Pts',(0.750193435981249,-1.,1.74080458267114));
#23158=CARTESIAN_POINT('Ctrl Pts',(0.751555614164482,-1.,1.74585086852502));
#23159=CARTESIAN_POINT('Ctrl Pts',(0.752797683531314,-1.,1.75095139468794));
#23160=CARTESIAN_POINT('Ctrl Pts',(0.754009254027828,-1.,1.75631083600019));
#23161=CARTESIAN_POINT('Ctrl Pts',(0.755220979974461,-1.,1.76197817240128));
#23162=CARTESIAN_POINT('Ctrl Pts',(0.75642189602781,-1.,1.76789396002998));
#23163=CARTESIAN_POINT('Ctrl Pts',(0.757578264077028,-1.,1.77394167108292));
#23164=CARTESIAN_POINT('Ctrl Pts',(0.758650626677518,-1.,1.77999411220945));
#23165=CARTESIAN_POINT('Ctrl Pts',(0.759614401110189,-1.,1.78596964884604));
#23166=CARTESIAN_POINT('Ctrl Pts',(0.760469555880749,-1.,1.7918581561088));
#23167=CARTESIAN_POINT('Ctrl Pts',(0.761229695230558,-1.,1.79768986997783));
#23168=CARTESIAN_POINT('Ctrl Pts',(0.761915336443547,-1.,1.80351583877342));
#23169=CARTESIAN_POINT('Ctrl Pts',(0.762546129463938,-1.,1.80938551463965));
#23170=CARTESIAN_POINT('Ctrl Pts',(0.763132003836634,-1.,1.8153211840553));
#23171=CARTESIAN_POINT('Ctrl Pts',(0.763673465462726,-1.,1.82131873145266));
#23172=CARTESIAN_POINT('Ctrl Pts',(0.764165902605995,-1.,1.82735991200065));
#23173=CARTESIAN_POINT('Ctrl Pts',(0.764602549687853,-1.,1.83342077227142));
#23174=CARTESIAN_POINT('Ctrl Pts',(0.764978057881737,-1.,1.83948181064835));
#23175=CARTESIAN_POINT('Ctrl Pts',(0.765291664862029,-1.,1.84553698875924));
#23176=CARTESIAN_POINT('Ctrl Pts',(0.765545710619062,-1.,1.85158945130063));
#23177=CARTESIAN_POINT('Ctrl Pts',(0.765744212909318,-1.,1.85764741390394));
#23178=CARTESIAN_POINT('Ctrl Pts',(0.765891519092547,-1.,1.86372027063312));
#23179=CARTESIAN_POINT('Ctrl Pts',(0.765990708546091,-1.,1.86981398314341));
#23180=CARTESIAN_POINT('Ctrl Pts',(0.766042837036744,-1.,1.87592888967883));
#23181=CARTESIAN_POINT('Ctrl Pts',(0.766047794851864,-1.,1.88206215302561));
#23182=CARTESIAN_POINT('Ctrl Pts',(0.766004837062091,-1.,1.88820926433409));
#23183=CARTESIAN_POINT('Ctrl Pts',(0.765913193856978,-1.,1.89436577771388));
#23184=CARTESIAN_POINT('Ctrl Pts',(0.765772772593386,-1.,1.90052930393596));
#23185=CARTESIAN_POINT('Ctrl Pts',(0.765584196937919,-1.,1.90669961402356));
#23186=CARTESIAN_POINT('Ctrl Pts',(0.765348465884722,-1.,1.91287765805169));
#23187=CARTESIAN_POINT('Ctrl Pts',(0.765066729667088,-1.,1.91906491634196));
#23188=CARTESIAN_POINT('Ctrl Pts',(0.764740025488211,-1.,1.92526263537048));
#23189=CARTESIAN_POINT('Ctrl Pts',(0.76436901067394,-1.,1.93147105496382));
#23190=CARTESIAN_POINT('Ctrl Pts',(0.763954049121458,-1.,1.93768964875886));
#23191=CARTESIAN_POINT('Ctrl Pts',(0.763495333538629,-1.,1.9439174661764));
#23192=CARTESIAN_POINT('Ctrl Pts',(0.762992990878769,-1.,1.95015342590024));
#23193=CARTESIAN_POINT('Ctrl Pts',(0.762447203806178,-1.,1.95639665309869));
#23194=CARTESIAN_POINT('Ctrl Pts',(0.761858300014423,-1.,1.96264672744186));
#23195=CARTESIAN_POINT('Ctrl Pts',(0.76122669048382,-1.,1.96890351582499));
#23196=CARTESIAN_POINT('Ctrl Pts',(0.760552825409757,-1.,1.97516705321494));
#23197=CARTESIAN_POINT('Ctrl Pts',(0.75983714745219,-1.,1.98143741418172));
#23198=CARTESIAN_POINT('Ctrl Pts',(0.759080037802488,-1.,1.98771456680874));
#23199=CARTESIAN_POINT('Ctrl Pts',(0.758281796766761,-1.,1.99399831098817));
#23200=CARTESIAN_POINT('Ctrl Pts',(0.757442676862724,-1.,2.00028834739178));
#23201=CARTESIAN_POINT('Ctrl Pts',(0.75656290464667,-1.,2.0065843158773));
#23202=CARTESIAN_POINT('Ctrl Pts',(0.755642704957865,-1.,2.01288584328084));
#23203=CARTESIAN_POINT('Ctrl Pts',(0.754682330722816,-1.,2.01919259405809));
#23204=CARTESIAN_POINT('Ctrl Pts',(0.753682061112768,-1.,2.02550428623313));
#23205=CARTESIAN_POINT('Ctrl Pts',(0.75264218048721,-1.,2.03182068456221));
#23206=CARTESIAN_POINT('Ctrl Pts',(0.751562963361115,-1.,2.03814160092099));
#23207=CARTESIAN_POINT('Ctrl Pts',(0.750444657875575,-1.,2.04446689147979));
#23208=CARTESIAN_POINT('Ctrl Pts',(0.749287468665046,-1.,2.05079645592154));
#23209=CARTESIAN_POINT('Ctrl Pts',(0.748091554183802,-1.,2.05713023031007));
#23210=CARTESIAN_POINT('Ctrl Pts',(0.747103932787919,-1.,2.06220058927826));
#23211=CARTESIAN_POINT('Ctrl Pts',(0.7463458715442,-1.,2.06600523016815));
#23212=CARTESIAN_POINT('Ctrl Pts',(0.745832791378367,-1.,2.06854248895728));
#23213=CARTESIAN_POINT('Ctrl Pts',(0.7455743247944,-1.,2.0698113262342));
#23214=CARTESIAN_POINT('',(0.61342227326009,-1.,2.11275013067528));
#23215=CARTESIAN_POINT('',(0.7455743247944,-1.,2.0698113262342));
#23216=CARTESIAN_POINT('',(0.383122945602004,-1.,1.7075470150345));
#23217=CARTESIAN_POINT('Ctrl Pts',(0.61342227326009,-1.,2.11275013067528));
#23218=CARTESIAN_POINT('Ctrl Pts',(0.6124673655618,-1.,2.11187554259986));
#23219=CARTESIAN_POINT('Ctrl Pts',(0.610560911689898,-1.,2.11012443807238));
#23220=CARTESIAN_POINT('Ctrl Pts',(0.607711315454876,-1.,2.1074919961518));
#23221=CARTESIAN_POINT('Ctrl Pts',(0.60393203073603,-1.,2.10397049886949));
#23222=CARTESIAN_POINT('Ctrl Pts',(0.599241616420533,-1.,2.0995493086477));
#23223=CARTESIAN_POINT('Ctrl Pts',(0.594585006052162,-1.,2.0951087622027));
#23224=CARTESIAN_POINT('Ctrl Pts',(0.589962365403406,-1.,2.09064881812129));
#23225=CARTESIAN_POINT('Ctrl Pts',(0.585373918991617,-1.,2.08616943727951));
#23226=CARTESIAN_POINT('Ctrl Pts',(0.580819952108063,-1.,2.08167059018418));
#23227=CARTESIAN_POINT('Ctrl Pts',(0.576300797416844,-1.,2.07715226767559));
#23228=CARTESIAN_POINT('Ctrl Pts',(0.571816823242602,-1.,2.07261449292824));
#23229=CARTESIAN_POINT('Ctrl Pts',(0.567368421181087,-1.,2.06805732997334));
#23230=CARTESIAN_POINT('Ctrl Pts',(0.562955993082261,-1.,2.06348090160589));
#23231=CARTESIAN_POINT('Ctrl Pts',(0.558579940185151,-1.,2.05888537756462));
#23232=CARTESIAN_POINT('Ctrl Pts',(0.554240657463906,-1.,2.05427091604413));
#23233=CARTESIAN_POINT('Ctrl Pts',(0.549938525150295,-1.,2.04963761077958));
#23234=CARTESIAN_POINT('Ctrl Pts',(0.54567390381743,-1.,2.04498544714588));
#23235=CARTESIAN_POINT('Ctrl Pts',(0.541447120615659,-1.,2.04031422690527));
#23236=CARTESIAN_POINT('Ctrl Pts',(0.537258489833262,-1.,2.03562362954037));
#23237=CARTESIAN_POINT('Ctrl Pts',(0.533108355132976,-1.,2.03091336214426));
#23238=CARTESIAN_POINT('Ctrl Pts',(0.528997127241914,-1.,2.0261832908329));
#23239=CARTESIAN_POINT('Ctrl Pts',(0.524925318333476,-1.,2.02143356304698));
#23240=CARTESIAN_POINT('Ctrl Pts',(0.52089359039937,-1.,2.01666477917286));
#23241=CARTESIAN_POINT('Ctrl Pts',(0.516902681728687,-1.,2.01187773939242));
#23242=CARTESIAN_POINT('Ctrl Pts',(0.512953306961792,-1.,2.00707309946949));
#23243=CARTESIAN_POINT('Ctrl Pts',(0.509046069886157,-1.,2.00225107134734));
#23244=CARTESIAN_POINT('Ctrl Pts',(0.505181361323026,-1.,1.99741107463572));
#23245=CARTESIAN_POINT('Ctrl Pts',(0.501359287727146,-1.,1.99255149126155));
#23246=CARTESIAN_POINT('Ctrl Pts',(0.497579909545574,-1.,1.98767044752932));
#23247=CARTESIAN_POINT('Ctrl Pts',(0.493843476541494,-1.,1.98276658761821));
#23248=CARTESIAN_POINT('Ctrl Pts',(0.490150627860952,-1.,1.97783973019229));
#23249=CARTESIAN_POINT('Ctrl Pts',(0.486502692907658,-1.,1.97289186263272));
#23250=CARTESIAN_POINT('Ctrl Pts',(0.48290166212069,-1.,1.96792703422362));
#23251=CARTESIAN_POINT('Ctrl Pts',(0.479349583074855,-1.,1.96294933055943));
#23252=CARTESIAN_POINT('Ctrl Pts',(0.475848034683176,-1.,1.95796111148177));
#23253=CARTESIAN_POINT('Ctrl Pts',(0.472397672264072,-1.,1.95296148278133));
#23254=CARTESIAN_POINT('Ctrl Pts',(0.468997482913135,-1.,1.94794381136514));
#23255=CARTESIAN_POINT('Ctrl Pts',(0.46564546202603,-1.,1.9428979419619));
#23256=CARTESIAN_POINT('Ctrl Pts',(0.462340031009056,-1.,1.93781486640821));
#23257=CARTESIAN_POINT('Ctrl Pts',(0.459081234547926,-1.,1.93269066517934));
#23258=CARTESIAN_POINT('Ctrl Pts',(0.45587200517437,-1.,1.92753067150476));
#23259=CARTESIAN_POINT('Ctrl Pts',(0.452719478359432,-1.,1.92235380648502));
#23260=CARTESIAN_POINT('Ctrl Pts',(0.449632260106662,-1.,1.91718342555755));
#23261=CARTESIAN_POINT('Ctrl Pts',(0.446617343485711,-1.,1.9120369998112));
#23262=CARTESIAN_POINT('Ctrl Pts',(0.44367755684915,-1.,1.90691756144898));
#23263=CARTESIAN_POINT('Ctrl Pts',(0.440807833704038,-1.,1.90180124389086));
#23264=CARTESIAN_POINT('Ctrl Pts',(0.437995003948244,-1.,1.89663648956466));
#23265=CARTESIAN_POINT('Ctrl Pts',(0.435225660963383,-1.,1.89136993975504));
#23266=CARTESIAN_POINT('Ctrl Pts',(0.432493038548748,-1.,1.88596913666793));
#23267=CARTESIAN_POINT('Ctrl Pts',(0.429803062482344,-1.,1.88044229001832));
#23268=CARTESIAN_POINT('Ctrl Pts',(0.427183828519102,-1.,1.87486989291484));
#23269=CARTESIAN_POINT('Ctrl Pts',(0.424678177291358,-1.,1.86937803944323));
#23270=CARTESIAN_POINT('Ctrl Pts',(0.422327307418275,-1.,1.86408083334028));
#23271=CARTESIAN_POINT('Ctrl Pts',(0.420157287975619,-1.,1.85903281096686));
#23272=CARTESIAN_POINT('Ctrl Pts',(0.418164129143534,-1.,1.85417632856234));
#23273=CARTESIAN_POINT('Ctrl Pts',(0.416300022038864,-1.,1.84929312929882));
#23274=CARTESIAN_POINT('Ctrl Pts',(0.41448743825434,-1.,1.8440575707371));
#23275=CARTESIAN_POINT('Ctrl Pts',(0.412633125322161,-1.,1.83808953475839));
#23276=CARTESIAN_POINT('Ctrl Pts',(0.410641256301674,-1.,1.83100408895216));
#23277=CARTESIAN_POINT('Ctrl Pts',(0.408428948108533,-1.,1.8224702267854));
#23278=CARTESIAN_POINT('Ctrl Pts',(0.405933518411838,-1.,1.81223801813988));
#23279=CARTESIAN_POINT('Ctrl Pts',(0.403107976170441,-1.,1.80012077176221));
#23280=CARTESIAN_POINT('Ctrl Pts',(0.39991940378308,-1.,1.78598826347533));
#23281=CARTESIAN_POINT('Ctrl Pts',(0.39634619612042,-1.,1.7697556004756));
#23282=CARTESIAN_POINT('Ctrl Pts',(0.392375812294307,-1.,1.75137405313962));
#23283=CARTESIAN_POINT('Ctrl Pts',(0.388877023509191,-1.,1.7349317097561));
#23284=CARTESIAN_POINT('Ctrl Pts',(0.38607079032701,-1.,1.72162022246158));
#23285=CARTESIAN_POINT('Ctrl Pts',(0.384119047315541,-1.,1.71231062891958));
#23286=CARTESIAN_POINT('Ctrl Pts',(0.383122945602004,-1.,1.7075470150345));
#23287=CARTESIAN_POINT('',(0.163289472382896,-1.,1.74236521665491));
#23288=CARTESIAN_POINT('Origin',(0.,-1.,0.));
#23289=CARTESIAN_POINT('',(0.0694764450219578,-1.,2.19890268624765));
#23290=CARTESIAN_POINT('Ctrl Pts',(0.163289472382896,-1.,1.74236521665491));
#23291=CARTESIAN_POINT('Ctrl Pts',(0.163814161002002,-1.,1.7472034950333));
#23292=CARTESIAN_POINT('Ctrl Pts',(0.164834765707158,-1.,1.75666056638427));
#23293=CARTESIAN_POINT('Ctrl Pts',(0.1662793551464,-1.,1.77018771684844));
#23294=CARTESIAN_POINT('Ctrl Pts',(0.168032772805197,-1.,1.7869064998507));
#23295=CARTESIAN_POINT('Ctrl Pts',(0.169936923904608,-1.,1.80561530629706));
#23296=CARTESIAN_POINT('Ctrl Pts',(0.171554770204119,-1.,1.82215766811545));
#23297=CARTESIAN_POINT('Ctrl Pts',(0.1728894428919,-1.,1.83658380527692));
#23298=CARTESIAN_POINT('Ctrl Pts',(0.173946627587731,-1.,1.8489811319852));
#23299=CARTESIAN_POINT('Ctrl Pts',(0.17473525927603,-1.,1.85948367088837));
#23300=CARTESIAN_POINT('Ctrl Pts',(0.175268337590757,-1.,1.86828349694799));
#23301=CARTESIAN_POINT('Ctrl Pts',(0.175563480746485,-1.,1.87563767773588));
#23302=CARTESIAN_POINT('Ctrl Pts',(0.175644148889698,-1.,1.88188663145367));
#23303=CARTESIAN_POINT('Ctrl Pts',(0.175538155840648,-1.,1.88742606273259));
#23304=CARTESIAN_POINT('Ctrl Pts',(0.175274276190844,-1.,1.892646301985));
#23305=CARTESIAN_POINT('Ctrl Pts',(0.174879405091263,-1.,1.89788101117132));
#23306=CARTESIAN_POINT('Ctrl Pts',(0.174375518661085,-1.,1.90335253862834));
#23307=CARTESIAN_POINT('Ctrl Pts',(0.173776635257816,-1.,1.90911693975267));
#23308=CARTESIAN_POINT('Ctrl Pts',(0.173090695383496,-1.,1.91511429159527));
#23309=CARTESIAN_POINT('Ctrl Pts',(0.172321621259513,-1.,1.9212233439798));
#23310=CARTESIAN_POINT('Ctrl Pts',(0.171471191532988,-1.,1.92731093582036));
#23311=CARTESIAN_POINT('Ctrl Pts',(0.170541253116201,-1.,1.93329183155539));
#23312=CARTESIAN_POINT('Ctrl Pts',(0.16953490481749,-1.,1.93915639211581));
#23313=CARTESIAN_POINT('Ctrl Pts',(0.168455741607556,-1.,1.94493757756931));
#23314=CARTESIAN_POINT('Ctrl Pts',(0.167307501784475,-1.,1.95069027794294));
#23315=CARTESIAN_POINT('Ctrl Pts',(0.166093592002812,-1.,1.9564675971873));
#23316=CARTESIAN_POINT('Ctrl Pts',(0.164816568920269,-1.,1.96229379940136));
#23317=CARTESIAN_POINT('Ctrl Pts',(0.163478185457734,-1.,1.96816512677967));
#23318=CARTESIAN_POINT('Ctrl Pts',(0.162079693556288,-1.,1.97406280235188));
#23319=CARTESIAN_POINT('Ctrl Pts',(0.160622060784611,-1.,1.97996195437559));
#23320=CARTESIAN_POINT('Ctrl Pts',(0.159106226437299,-1.,1.98584238283292));
#23321=CARTESIAN_POINT('Ctrl Pts',(0.157533331459227,-1.,1.99169810931908));
#23322=CARTESIAN_POINT('Ctrl Pts',(0.155904629548783,-1.,1.99753284771497));
#23323=CARTESIAN_POINT('Ctrl Pts',(0.154221403049722,-1.,2.00335565310543));
#23324=CARTESIAN_POINT('Ctrl Pts',(0.152484883621449,-1.,2.00917680318424));
#23325=CARTESIAN_POINT('Ctrl Pts',(0.150696157673078,-1.,2.01500291940238));
#23326=CARTESIAN_POINT('Ctrl Pts',(0.148856124775337,-1.,2.02083464969894));
#23327=CARTESIAN_POINT('Ctrl Pts',(0.146965557332583,-1.,2.02666926182017));
#23328=CARTESIAN_POINT('Ctrl Pts',(0.145025140186057,-1.,2.03250223739942));
#23329=CARTESIAN_POINT('Ctrl Pts',(0.143035515058208,-1.,2.03832911025912));
#23330=CARTESIAN_POINT('Ctrl Pts',(0.140997332152546,-1.,2.04414757947916));
#23331=CARTESIAN_POINT('Ctrl Pts',(0.138911255368966,-1.,2.04995762001328));
#23332=CARTESIAN_POINT('Ctrl Pts',(0.136777941218043,-1.,2.05576044414264));
#23333=CARTESIAN_POINT('Ctrl Pts',(0.134598026192106,-1.,2.06155781517842));
#23334=CARTESIAN_POINT('Ctrl Pts',(0.13237211154771,-1.,2.06735123910326));
#23335=CARTESIAN_POINT('Ctrl Pts',(0.130100748328403,-1.,2.07314114713063));
#23336=CARTESIAN_POINT('Ctrl Pts',(0.12778444527612,-1.,2.07892715110987));
#23337=CARTESIAN_POINT('Ctrl Pts',(0.125423679412061,-1.,2.08470840653643));
#23338=CARTESIAN_POINT('Ctrl Pts',(0.123018905621083,-1.,2.09048392424825));
#23339=CARTESIAN_POINT('Ctrl Pts',(0.120570567965122,-1.,2.0962529286773));
#23340=CARTESIAN_POINT('Ctrl Pts',(0.118079107988355,-1.,2.102015121329));
#23341=CARTESIAN_POINT('Ctrl Pts',(0.115544957687926,-1.,2.10777050261309));
#23342=CARTESIAN_POINT('Ctrl Pts',(0.112968534419737,-1.,2.11351924490306));
#23343=CARTESIAN_POINT('Ctrl Pts',(0.110350236135025,-1.,2.11926155590865));
#23344=CARTESIAN_POINT('Ctrl Pts',(0.10769043523109,-1.,2.12499752307));
#23345=CARTESIAN_POINT('Ctrl Pts',(0.104989479152739,-1.,2.13072704887293));
#23346=CARTESIAN_POINT('Ctrl Pts',(0.1022477005561,-1.,2.13644992667165));
#23347=CARTESIAN_POINT('Ctrl Pts',(0.0994654261990913,-1.,2.14216588396025));
#23348=CARTESIAN_POINT('Ctrl Pts',(0.0966429852305456,-1.,2.14787463531795));
#23349=CARTESIAN_POINT('Ctrl Pts',(0.0937807218867641,-1.,2.1535759397817));
#23350=CARTESIAN_POINT('Ctrl Pts',(0.0908789888107263,-1.,2.15926961544516));
#23351=CARTESIAN_POINT('Ctrl Pts',(0.087938129138692,-1.,2.16495552645014));
#23352=CARTESIAN_POINT('Ctrl Pts',(0.084958462083537,-1.,2.17063357870952));
#23353=CARTESIAN_POINT('Ctrl Pts',(0.0819402680872763,-1.,2.176303712113));
#23354=CARTESIAN_POINT('Ctrl Pts',(0.078883772768524,-1.,2.18196589448887));
#23355=CARTESIAN_POINT('Ctrl Pts',(0.0757891465836145,-1.,2.1876201139953));
#23356=CARTESIAN_POINT('Ctrl Pts',(0.0732830357306722,-1.,2.19213712013662));
#23357=CARTESIAN_POINT('Ctrl Pts',(0.0713863779526151,-1.,2.19552129484002));
#23358=CARTESIAN_POINT('Ctrl Pts',(0.0701143536325487,-1.,2.19777582085423));
#23359=CARTESIAN_POINT('Ctrl Pts',(0.0694764450219578,-1.,2.19890268624765));
#23360=CARTESIAN_POINT('',(-0.0694764450219586,-1.,2.19890268624765));
#23361=CARTESIAN_POINT('',(0.0694764450219578,-1.,2.19890268624765));
#23362=CARTESIAN_POINT('',(-0.163289472382896,-1.,1.74236521665491));
#23363=CARTESIAN_POINT('Ctrl Pts',(-0.0694764450219586,-1.,2.19890268624765));
#23364=CARTESIAN_POINT('Ctrl Pts',(-0.0701143536324929,-1.,2.19777582085261));
#23365=CARTESIAN_POINT('Ctrl Pts',(-0.071386377952463,-1.,2.19552129483562));
#23366=CARTESIAN_POINT('Ctrl Pts',(-0.0732830357304279,-1.,2.19213712012956));
#23367=CARTESIAN_POINT('Ctrl Pts',(-0.0757891465833414,-1.,2.1876201139874));
#23368=CARTESIAN_POINT('Ctrl Pts',(-0.078883772768323,-1.,2.18196589448304));
#23369=CARTESIAN_POINT('Ctrl Pts',(-0.0819402680871942,-1.,2.1763037121106));
#23370=CARTESIAN_POINT('Ctrl Pts',(-0.0849584620835646,-1.,2.17063357871031));
#23371=CARTESIAN_POINT('Ctrl Pts',(-0.0879381291387825,-1.,2.16495552645275));
#23372=CARTESIAN_POINT('Ctrl Pts',(-0.0908789888108269,-1.,2.15926961544808));
#23373=CARTESIAN_POINT('Ctrl Pts',(-0.0937807218868348,-1.,2.15357593978377));
#23374=CARTESIAN_POINT('Ctrl Pts',(-0.0966429852305691,-1.,2.14787463531864));
#23375=CARTESIAN_POINT('Ctrl Pts',(-0.0994654261990745,-1.,2.14216588395974));
#23376=CARTESIAN_POINT('Ctrl Pts',(-0.102247700556064,-1.,2.13644992667052));
#23377=CARTESIAN_POINT('Ctrl Pts',(-0.104989479152703,-1.,2.1307270488718));
#23378=CARTESIAN_POINT('Ctrl Pts',(-0.107690435231068,-1.,2.12499752306927));
#23379=CARTESIAN_POINT('Ctrl Pts',(-0.11035023613502,-1.,2.11926155590849));
#23380=CARTESIAN_POINT('Ctrl Pts',(-0.112968534419746,-1.,2.11351924490335));
#23381=CARTESIAN_POINT('Ctrl Pts',(-0.115544957687941,-1.,2.10777050261359));
#23382=CARTESIAN_POINT('Ctrl Pts',(-0.118079107988368,-1.,2.10201512132945));
#23383=CARTESIAN_POINT('Ctrl Pts',(-0.120570567965129,-1.,2.09625292867756));
#23384=CARTESIAN_POINT('Ctrl Pts',(-0.123018905621083,-1.,2.09048392424826));
#23385=CARTESIAN_POINT('Ctrl Pts',(-0.125423679412058,-1.,2.08470840653628));
#23386=CARTESIAN_POINT('Ctrl Pts',(-0.127784445276116,-1.,2.07892715110967));
#23387=CARTESIAN_POINT('Ctrl Pts',(-0.130100748328401,-1.,2.07314114713047));
#23388=CARTESIAN_POINT('Ctrl Pts',(-0.13237211154771,-1.,2.06735123910319));
#23389=CARTESIAN_POINT('Ctrl Pts',(-0.134598026192107,-1.,2.06155781517844));
#23390=CARTESIAN_POINT('Ctrl Pts',(-0.136777941218044,-1.,2.0557604441427));
#23391=CARTESIAN_POINT('Ctrl Pts',(-0.138911255368966,-1.,2.04995762001333));
#23392=CARTESIAN_POINT('Ctrl Pts',(-0.140997332152546,-1.,2.04414757947919));
#23393=CARTESIAN_POINT('Ctrl Pts',(-0.143035515058208,-1.,2.03832911025913));
#23394=CARTESIAN_POINT('Ctrl Pts',(-0.145025140186058,-1.,2.03250223739941));
#23395=CARTESIAN_POINT('Ctrl Pts',(-0.146965557332586,-1.,2.02666926182017));
#23396=CARTESIAN_POINT('Ctrl Pts',(-0.148856124775343,-1.,2.02083464969897));
#23397=CARTESIAN_POINT('Ctrl Pts',(-0.150696157673084,-1.,2.01500291940243));
#23398=CARTESIAN_POINT('Ctrl Pts',(-0.152484883621452,-1.,2.00917680318426));
#23399=CARTESIAN_POINT('Ctrl Pts',(-0.154221403049719,-1.,2.00335565310539));
#23400=CARTESIAN_POINT('Ctrl Pts',(-0.155904629548775,-1.,1.99753284771487));
#23401=CARTESIAN_POINT('Ctrl Pts',(-0.157533331459215,-1.,1.99169810931893));
#23402=CARTESIAN_POINT('Ctrl Pts',(-0.159106226437289,-1.,1.98584238283279));
#23403=CARTESIAN_POINT('Ctrl Pts',(-0.16062206078461,-1.,1.97996195437557));
#23404=CARTESIAN_POINT('Ctrl Pts',(-0.162079693556302,-1.,1.97406280235204));
#23405=CARTESIAN_POINT('Ctrl Pts',(-0.16347818545776,-1.,1.96816512678));
#23406=CARTESIAN_POINT('Ctrl Pts',(-0.1648165689203,-1.,1.96229379940174));
#23407=CARTESIAN_POINT('Ctrl Pts',(-0.166093592002833,-1.,1.95646759718755));
#23408=CARTESIAN_POINT('Ctrl Pts',(-0.167307501784469,-1.,1.95069027794286));
#23409=CARTESIAN_POINT('Ctrl Pts',(-0.168455741607516,-1.,1.94493757756879));
#23410=CARTESIAN_POINT('Ctrl Pts',(-0.169534904817425,-1.,1.93915639211497));
#23411=CARTESIAN_POINT('Ctrl Pts',(-0.170541253116136,-1.,1.93329183155455));
#23412=CARTESIAN_POINT('Ctrl Pts',(-0.17147119153296,-1.,1.92731093582));
#23413=CARTESIAN_POINT('Ctrl Pts',(-0.172321621259557,-1.,1.92122334398034));
#23414=CARTESIAN_POINT('Ctrl Pts',(-0.173090695383619,-1.,1.91511429159681));
#23415=CARTESIAN_POINT('Ctrl Pts',(-0.173776635257984,-1.,1.90911693975475));
#23416=CARTESIAN_POINT('Ctrl Pts',(-0.174375518661222,-1.,1.90335253863003));
#23417=CARTESIAN_POINT('Ctrl Pts',(-0.174879405091277,-1.,1.89788101117148));
#23418=CARTESIAN_POINT('Ctrl Pts',(-0.175274276190664,-1.,1.89264630198279));
#23419=CARTESIAN_POINT('Ctrl Pts',(-0.175538155840286,-1.,1.88742606272818));
#23420=CARTESIAN_POINT('Ctrl Pts',(-0.175644148889271,-1.,1.88188663144846));
#23421=CARTESIAN_POINT('Ctrl Pts',(-0.175563480746206,-1.,1.87563767773249));
#23422=CARTESIAN_POINT('Ctrl Pts',(-0.175268337590901,-1.,1.86828349694972));
#23423=CARTESIAN_POINT('Ctrl Pts',(-0.174735259276856,-1.,1.85948367089838));
#23424=CARTESIAN_POINT('Ctrl Pts',(-0.173946627589401,-1.,1.84898113200543));
#23425=CARTESIAN_POINT('Ctrl Pts',(-0.17288944289442,-1.,1.83658380530747));
#23426=CARTESIAN_POINT('Ctrl Pts',(-0.171554770207306,-1.,1.82215766815414));
#23427=CARTESIAN_POINT('Ctrl Pts',(-0.169936923908078,-1.,1.80561530633924));
#23428=CARTESIAN_POINT('Ctrl Pts',(-0.16803277280837,-1.,1.78690649988931));
#23429=CARTESIAN_POINT('Ctrl Pts',(-0.166279355148738,-1.,1.77018771687692));
#23430=CARTESIAN_POINT('Ctrl Pts',(-0.164834765708484,-1.,1.75666056640041));
#23431=CARTESIAN_POINT('Ctrl Pts',(-0.163814161002474,-1.,1.74720349503904));
#23432=CARTESIAN_POINT('Ctrl Pts',(-0.163289472382896,-1.,1.74236521665491));
#23433=CARTESIAN_POINT('',(-0.383122945602004,-1.,1.7075470150345));
#23434=CARTESIAN_POINT('Origin',(0.,-1.,0.));
#23435=CARTESIAN_POINT('',(-0.61342227326009,-1.,2.11275013067528));
#23436=CARTESIAN_POINT('Ctrl Pts',(-0.383122945602004,-1.,1.7075470150345));
#23437=CARTESIAN_POINT('Ctrl Pts',(-0.384119047314215,-1.,1.71231062891398));
#23438=CARTESIAN_POINT('Ctrl Pts',(-0.386070790323281,-1.,1.72162022244582));
#23439=CARTESIAN_POINT('Ctrl Pts',(-0.388877023502615,-1.,1.73493170972829));
#23440=CARTESIAN_POINT('Ctrl Pts',(-0.392375812285395,-1.,1.75137405310193));
#23441=CARTESIAN_POINT('Ctrl Pts',(-0.396346196110688,-1.,1.76975560043442));
#23442=CARTESIAN_POINT('Ctrl Pts',(-0.399919403774155,-1.,1.78598826343754));
#23443=CARTESIAN_POINT('Ctrl Pts',(-0.403107976163396,-1.,1.80012077173238));
#23444=CARTESIAN_POINT('Ctrl Pts',(-0.405933518407175,-1.,1.81223801812013));
#23445=CARTESIAN_POINT('Ctrl Pts',(-0.408428948106227,-1.,1.82247022677562));
#23446=CARTESIAN_POINT('Ctrl Pts',(-0.410641256301276,-1.,1.83100408895047));
#23447=CARTESIAN_POINT('Ctrl Pts',(-0.412633125322945,-1.,1.8380895347617));
#23448=CARTESIAN_POINT('Ctrl Pts',(-0.414487438255542,-1.,1.84405757074218));
#23449=CARTESIAN_POINT('Ctrl Pts',(-0.416300022039885,-1.,1.84929312930314));
#23450=CARTESIAN_POINT('Ctrl Pts',(-0.418164129144045,-1.,1.8541763285645));
#23451=CARTESIAN_POINT('Ctrl Pts',(-0.420157287975583,-1.,1.8590328109667));
#23452=CARTESIAN_POINT('Ctrl Pts',(-0.422327307417885,-1.,1.86408083333863));
#23453=CARTESIAN_POINT('Ctrl Pts',(-0.424678177290876,-1.,1.8693780394412));
#23454=CARTESIAN_POINT('Ctrl Pts',(-0.427183828518743,-1.,1.87486989291333));
#23455=CARTESIAN_POINT('Ctrl Pts',(-0.429803062482217,-1.,1.88044229001778));
#23456=CARTESIAN_POINT('Ctrl Pts',(-0.432493038548833,-1.,1.88596913666828));
#23457=CARTESIAN_POINT('Ctrl Pts',(-0.43522566096358,-1.,1.89136993975585));
#23458=CARTESIAN_POINT('Ctrl Pts',(-0.437995003948443,-1.,1.89663648956549));
#23459=CARTESIAN_POINT('Ctrl Pts',(-0.440807833704161,-1.,1.90180124389137));
#23460=CARTESIAN_POINT('Ctrl Pts',(-0.44367755684917,-1.,1.90691756144906));
#23461=CARTESIAN_POINT('Ctrl Pts',(-0.446617343485651,-1.,1.91203699981095));
#23462=CARTESIAN_POINT('Ctrl Pts',(-0.449632260106572,-1.,1.91718342555717));
#23463=CARTESIAN_POINT('Ctrl Pts',(-0.452719478359356,-1.,1.9223538064847));
#23464=CARTESIAN_POINT('Ctrl Pts',(-0.455872005174335,-1.,1.92753067150461));
#23465=CARTESIAN_POINT('Ctrl Pts',(-0.459081234547931,-1.,1.93269066517936));
#23466=CARTESIAN_POINT('Ctrl Pts',(-0.462340031009087,-1.,1.93781486640834));
#23467=CARTESIAN_POINT('Ctrl Pts',(-0.465645462026065,-1.,1.94289794196205));
#23468=CARTESIAN_POINT('Ctrl Pts',(-0.468997482913158,-1.,1.94794381136524));
#23469=CARTESIAN_POINT('Ctrl Pts',(-0.47239767226408,-1.,1.95296148278136));
#23470=CARTESIAN_POINT('Ctrl Pts',(-0.475848034683172,-1.,1.95796111148175));
#23471=CARTESIAN_POINT('Ctrl Pts',(-0.479349583074846,-1.,1.96294933055938));
#23472=CARTESIAN_POINT('Ctrl Pts',(-0.482901662120687,-1.,1.96792703422358));
#23473=CARTESIAN_POINT('Ctrl Pts',(-0.486502692907661,-1.,1.97289186263272));
#23474=CARTESIAN_POINT('Ctrl Pts',(-0.490150627860955,-1.,1.97783973019229));
#23475=CARTESIAN_POINT('Ctrl Pts',(-0.493843476541492,-1.,1.9827665876182));
#23476=CARTESIAN_POINT('Ctrl Pts',(-0.497579909545564,-1.,1.98767044752929));
#23477=CARTESIAN_POINT('Ctrl Pts',(-0.501359287727129,-1.,1.9925514912615));
#23478=CARTESIAN_POINT('Ctrl Pts',(-0.505181361323011,-1.,1.99741107463567));
#23479=CARTESIAN_POINT('Ctrl Pts',(-0.509046069886152,-1.,2.00225107134733));
#23480=CARTESIAN_POINT('Ctrl Pts',(-0.512953306961814,-1.,2.00707309946955));
#23481=CARTESIAN_POINT('Ctrl Pts',(-0.516902681728733,-1.,2.01187773939257));
#23482=CARTESIAN_POINT('Ctrl Pts',(-0.520893590399428,-1.,2.01666477917305));
#23483=CARTESIAN_POINT('Ctrl Pts',(-0.524925318333518,-1.,2.02143356304712));
#23484=CARTESIAN_POINT('Ctrl Pts',(-0.528997127241911,-1.,2.02618329083289));
#23485=CARTESIAN_POINT('Ctrl Pts',(-0.533108355132905,-1.,2.03091336214401));
#23486=CARTESIAN_POINT('Ctrl Pts',(-0.537258489833134,-1.,2.03562362953993));
#23487=CARTESIAN_POINT('Ctrl Pts',(-0.54144712061552,-1.,2.0403142269048));
#23488=CARTESIAN_POINT('Ctrl Pts',(-0.545673903817348,-1.,2.0449854471456));
#23489=CARTESIAN_POINT('Ctrl Pts',(-0.549938525150342,-1.,2.04963761077974));
#23490=CARTESIAN_POINT('Ctrl Pts',(-0.55424065746411,-1.,2.05427091604482));
#23491=CARTESIAN_POINT('Ctrl Pts',(-0.558579940185467,-1.,2.05888537756571));
#23492=CARTESIAN_POINT('Ctrl Pts',(-0.562955993082574,-1.,2.06348090160697));
#23493=CARTESIAN_POINT('Ctrl Pts',(-0.567368421181229,-1.,2.06805732997383));
#23494=CARTESIAN_POINT('Ctrl Pts',(-0.571816823242411,-1.,2.07261449292757));
#23495=CARTESIAN_POINT('Ctrl Pts',(-0.576300797416275,-1.,2.07715226767361));
#23496=CARTESIAN_POINT('Ctrl Pts',(-0.580819952107257,-1.,2.08167059018138));
#23497=CARTESIAN_POINT('Ctrl Pts',(-0.585373918990895,-1.,2.086169437277));
#23498=CARTESIAN_POINT('Ctrl Pts',(-0.589962365403189,-1.,2.09064881812053));
#23499=CARTESIAN_POINT('Ctrl Pts',(-0.594585006052824,-1.,2.09510876220501));
#23500=CARTESIAN_POINT('Ctrl Pts',(-0.599241616422144,-1.,2.09954930865331));
#23501=CARTESIAN_POINT('Ctrl Pts',(-0.603932030738212,-1.,2.10397049887709));
#23502=CARTESIAN_POINT('Ctrl Pts',(-0.607711315456826,-1.,2.10749199615859));
#23503=CARTESIAN_POINT('Ctrl Pts',(-0.610560911691113,-1.,2.11012443807661));
#23504=CARTESIAN_POINT('Ctrl Pts',(-0.61246736556225,-1.,2.11187554260142));
#23505=CARTESIAN_POINT('Ctrl Pts',(-0.61342227326009,-1.,2.11275013067528));
#23506=CARTESIAN_POINT('',(-0.745574324794401,-1.,2.0698113262342));
#23507=CARTESIAN_POINT('',(-0.61342227326009,-1.,2.11275013067528));
#23508=CARTESIAN_POINT('',(-0.693717979106306,-1.,1.60662857109684));
#23509=CARTESIAN_POINT('Ctrl Pts',(-0.745574324794401,-1.,2.0698113262342));
#23510=CARTESIAN_POINT('Ctrl Pts',(-0.74583279137781,-1.,2.06854248895575));
#23511=CARTESIAN_POINT('Ctrl Pts',(-0.746345871542696,-1.,2.06600523016401));
#23512=CARTESIAN_POINT('Ctrl Pts',(-0.747103932785504,-1.,2.06220058927162));
#23513=CARTESIAN_POINT('Ctrl Pts',(-0.748091554181101,-1.,2.05713023030263));
#23514=CARTESIAN_POINT('Ctrl Pts',(-0.749287468663053,-1.,2.05079645591606));
#23515=CARTESIAN_POINT('Ctrl Pts',(-0.750444657874758,-1.,2.04446689147754));
#23516=CARTESIAN_POINT('Ctrl Pts',(-0.751562963361384,-1.,2.03814160092173));
#23517=CARTESIAN_POINT('Ctrl Pts',(-0.752642180488104,-1.,2.03182068456467));
#23518=CARTESIAN_POINT('Ctrl Pts',(-0.753682061113766,-1.,2.02550428623587));
#23519=CARTESIAN_POINT('Ctrl Pts',(-0.75468233072352,-1.,2.01919259406003));
#23520=CARTESIAN_POINT('Ctrl Pts',(-0.7556427049581,-1.,2.01288584328149));
#23521=CARTESIAN_POINT('Ctrl Pts',(-0.756562904646496,-1.,2.00658431587682));
#23522=CARTESIAN_POINT('Ctrl Pts',(-0.757442676862341,-1.,2.00028834739072));
#23523=CARTESIAN_POINT('Ctrl Pts',(-0.758281796766377,-1.,1.9939983109871));
#23524=CARTESIAN_POINT('Ctrl Pts',(-0.759080037802243,-1.,1.98771456680806));
#23525=CARTESIAN_POINT('Ctrl Pts',(-0.759837147452135,-1.,1.98143741418156));
#23526=CARTESIAN_POINT('Ctrl Pts',(-0.760552825409855,-1.,1.97516705321521));
#23527=CARTESIAN_POINT('Ctrl Pts',(-0.761226690483986,-1.,1.96890351582545));
#23528=CARTESIAN_POINT('Ctrl Pts',(-0.761858300014575,-1.,1.96264672744229));
#23529=CARTESIAN_POINT('Ctrl Pts',(-0.762447203806263,-1.,1.95639665309893));
#23530=CARTESIAN_POINT('Ctrl Pts',(-0.762992990878774,-1.,1.95015342590025));
#23531=CARTESIAN_POINT('Ctrl Pts',(-0.76349533353858,-1.,1.94391746617626));
#23532=CARTESIAN_POINT('Ctrl Pts',(-0.763954049121393,-1.,1.93768964875867));
#23533=CARTESIAN_POINT('Ctrl Pts',(-0.764369010673889,-1.,1.93147105496367));
#23534=CARTESIAN_POINT('Ctrl Pts',(-0.764740025488189,-1.,1.92526263537041));
#23535=CARTESIAN_POINT('Ctrl Pts',(-0.765066729667095,-1.,1.91906491634197));
#23536=CARTESIAN_POINT('Ctrl Pts',(-0.765348465884739,-1.,1.91287765805174));
#23537=CARTESIAN_POINT('Ctrl Pts',(-0.765584196937936,-1.,1.90669961402362));
#23538=CARTESIAN_POINT('Ctrl Pts',(-0.765772772593395,-1.,1.90052930393599));
#23539=CARTESIAN_POINT('Ctrl Pts',(-0.765913193856979,-1.,1.89436577771389));
#23540=CARTESIAN_POINT('Ctrl Pts',(-0.76600483706209,-1.,1.88820926433409));
#23541=CARTESIAN_POINT('Ctrl Pts',(-0.766047794851869,-1.,1.88206215302561));
#23542=CARTESIAN_POINT('Ctrl Pts',(-0.766042837036759,-1.,1.87592888967886));
#23543=CARTESIAN_POINT('Ctrl Pts',(-0.765990708546111,-1.,1.86981398314345));
#23544=CARTESIAN_POINT('Ctrl Pts',(-0.765891519092557,-1.,1.86372027063314));
#23545=CARTESIAN_POINT('Ctrl Pts',(-0.765744212909305,-1.,1.85764741390391));
#23546=CARTESIAN_POINT('Ctrl Pts',(-0.765545710619023,-1.,1.85158945130054));
#23547=CARTESIAN_POINT('Ctrl Pts',(-0.765291664861971,-1.,1.8455369887591));
#23548=CARTESIAN_POINT('Ctrl Pts',(-0.764978057881687,-1.,1.83948181064823));
#23549=CARTESIAN_POINT('Ctrl Pts',(-0.764602549687845,-1.,1.8334207722714));
#23550=CARTESIAN_POINT('Ctrl Pts',(-0.764165902606055,-1.,1.8273599120008));
#23551=CARTESIAN_POINT('Ctrl Pts',(-0.763673465462854,-1.,1.82131873145297));
#23552=CARTESIAN_POINT('Ctrl Pts',(-0.763132003836783,-1.,1.81532118405566));
#23553=CARTESIAN_POINT('Ctrl Pts',(-0.762546129464036,-1.,1.80938551463989));
#23554=CARTESIAN_POINT('Ctrl Pts',(-0.761915336443516,-1.,1.80351583877334));
#23555=CARTESIAN_POINT('Ctrl Pts',(-0.761229695230359,-1.,1.79768986997735));
#23556=CARTESIAN_POINT('Ctrl Pts',(-0.760469555880425,-1.,1.79185815610802));
#23557=CARTESIAN_POINT('Ctrl Pts',(-0.759614401109868,-1.,1.78596964884526));
#23558=CARTESIAN_POINT('Ctrl Pts',(-0.75865062667738,-1.,1.77999411220912));
#23559=CARTESIAN_POINT('Ctrl Pts',(-0.757578264077238,-1.,1.77394167108342));
#23560=CARTESIAN_POINT('Ctrl Pts',(-0.756421896028403,-1.,1.76789396003141));
#23561=CARTESIAN_POINT('Ctrl Pts',(-0.755220979975262,-1.,1.7619781724032));
#23562=CARTESIAN_POINT('Ctrl Pts',(-0.75400925402848,-1.,1.75631083600175));
#23563=CARTESIAN_POINT('Ctrl Pts',(-0.752797683531377,-1.,1.75095139468809));
#23564=CARTESIAN_POINT('Ctrl Pts',(-0.751555614163629,-1.,1.74585086852298));
#23565=CARTESIAN_POINT('Ctrl Pts',(-0.75019343597954,-1.,1.74080458266705));
#23566=CARTESIAN_POINT('Ctrl Pts',(-0.748582462954855,-1.,1.73550351679848));
#23567=CARTESIAN_POINT('Ctrl Pts',(-0.746574710096436,-1.,1.72958533647399));
#23568=CARTESIAN_POINT('Ctrl Pts',(-0.744021445433764,-1.,1.7226822991693));
#23569=CARTESIAN_POINT('Ctrl Pts',(-0.740795162032088,-1.,1.71447789751927));
#23570=CARTESIAN_POINT('Ctrl Pts',(-0.736799665724771,-1.,1.70473309006121));
#23571=CARTESIAN_POINT('Ctrl Pts',(-0.731963238697195,-1.,1.69326921975743));
#23572=CARTESIAN_POINT('Ctrl Pts',(-0.726235967997433,-1.,1.67996158455503));
#23573=CARTESIAN_POINT('Ctrl Pts',(-0.719585433804282,-1.,1.6647288055568));
#23574=CARTESIAN_POINT('Ctrl Pts',(-0.711993139355394,-1.,1.64752408832016));
#23575=CARTESIAN_POINT('Ctrl Pts',(-0.705159151988319,-1.,1.63216541664676));
#23576=CARTESIAN_POINT('Ctrl Pts',(-0.699605146405088,-1.,1.61974673472612));
#23577=CARTESIAN_POINT('Ctrl Pts',(-0.695712097881194,-1.,1.61106790958151));
#23578=CARTESIAN_POINT('Ctrl Pts',(-0.693717979106306,-1.,1.60662857109684));
#23579=CARTESIAN_POINT('',(-0.892032620296855,-1.,1.5055822144029));
#23580=CARTESIAN_POINT('Origin',(0.,-1.,0.));
#23581=CARTESIAN_POINT('',(-1.23627494547115,-1.,1.81978687191668));
#23582=CARTESIAN_POINT('Ctrl Pts',(-0.892032620296855,-1.,1.5055822144029));
#23583=CARTESIAN_POINT('Ctrl Pts',(-0.894452006964543,-1.,1.50980486806688));
#23584=CARTESIAN_POINT('Ctrl Pts',(-0.899185047483511,-1.,1.51805569590094));
#23585=CARTESIAN_POINT('Ctrl Pts',(-0.905967409625651,-1.,1.52984849887993));
#23586=CARTESIAN_POINT('Ctrl Pts',(-0.914375919026456,-1.,1.54440491149498));
#23587=CARTESIAN_POINT('Ctrl Pts',(-0.923832188944341,-1.,1.56065988578893));
#23588=CARTESIAN_POINT('Ctrl Pts',(-0.932246680108685,-1.,1.57499388382243));
#23589=CARTESIAN_POINT('Ctrl Pts',(-0.939646377893399,-1.,1.58744937487176));
#23590=CARTESIAN_POINT('Ctrl Pts',(-0.946078063315257,-1.,1.59810042043673));
#23591=CARTESIAN_POINT('Ctrl Pts',(-0.951613284356035,-1.,1.60706069896936));
#23592=CARTESIAN_POINT('Ctrl Pts',(-0.956354422920671,-1.,1.61449324337085));
#23593=CARTESIAN_POINT('Ctrl Pts',(-0.960438326101729,-1.,1.62061638140221));
#23594=CARTESIAN_POINT('Ctrl Pts',(-0.964046107040536,-1.,1.62571930670187));
#23595=CARTESIAN_POINT('Ctrl Pts',(-0.967387853230345,-1.,1.63013849959461));
#23596=CARTESIAN_POINT('Ctrl Pts',(-0.970669715997509,-1.,1.63420665729798));
#23597=CARTESIAN_POINT('Ctrl Pts',(-0.974066058287418,-1.,1.63820952658144));
#23598=CARTESIAN_POINT('Ctrl Pts',(-0.977689794119416,-1.,1.64233990826687));
#23599=CARTESIAN_POINT('Ctrl Pts',(-0.981562530939489,-1.,1.64665139190656));
#23600=CARTESIAN_POINT('Ctrl Pts',(-0.985642622920821,-1.,1.65110016612638));
#23601=CARTESIAN_POINT('Ctrl Pts',(-0.989855627854165,-1.,1.65559044289699));
#23602=CARTESIAN_POINT('Ctrl Pts',(-0.994121836661306,-1.,1.66001553809947));
#23603=CARTESIAN_POINT('Ctrl Pts',(-0.998389654952758,-1.,1.66430758030376));
#23604=CARTESIAN_POINT('Ctrl Pts',(-1.00265091003727,-1.,1.66846059277303));
#23605=CARTESIAN_POINT('Ctrl Pts',(-1.00692206696414,-1.,1.67250335383293));
#23606=CARTESIAN_POINT('Ctrl Pts',(-1.01123236493511,-1.,1.67648246776464));
#23607=CARTESIAN_POINT('Ctrl Pts',(-1.01561026162773,-1.,1.68044289894798));
#23608=CARTESIAN_POINT('Ctrl Pts',(-1.02006795074201,-1.,1.68440578021706));
#23609=CARTESIAN_POINT('Ctrl Pts',(-1.02460180535255,-1.,1.68836910178447));
#23610=CARTESIAN_POINT('Ctrl Pts',(-1.02919977579147,-1.,1.69231840863458));
#23611=CARTESIAN_POINT('Ctrl Pts',(-1.03384646003588,-1.,1.69623414782771));
#23612=CARTESIAN_POINT('Ctrl Pts',(-1.03852922490789,-1.,1.70010052930962));
#23613=CARTESIAN_POINT('Ctrl Pts',(-1.04324363334554,-1.,1.70391338707982));
#23614=CARTESIAN_POINT('Ctrl Pts',(-1.04799085404995,-1.,1.70767646263649));
#23615=CARTESIAN_POINT('Ctrl Pts',(-1.05277517202855,-1.,1.71139783543989));
#23616=CARTESIAN_POINT('Ctrl Pts',(-1.05760163192479,-1.,1.7150865442702));
#23617=CARTESIAN_POINT('Ctrl Pts',(-1.06247324680647,-1.,1.71874858456904));
#23618=CARTESIAN_POINT('Ctrl Pts',(-1.06738966975462,-1.,1.72238500928453));
#23619=CARTESIAN_POINT('Ctrl Pts',(-1.07234866990252,-1.,1.72599406198488));
#23620=CARTESIAN_POINT('Ctrl Pts',(-1.0773470373727,-1.,1.72957248977424));
#23621=CARTESIAN_POINT('Ctrl Pts',(-1.08238162784749,-1.,1.73311705663407));
#23622=CARTESIAN_POINT('Ctrl Pts',(-1.08745056285427,-1.,1.73662628326091));
#23623=CARTESIAN_POINT('Ctrl Pts',(-1.09255329056493,-1.,1.74010053962247));
#23624=CARTESIAN_POINT('Ctrl Pts',(-1.09768999241225,-1.,1.74354119236208));
#23625=CARTESIAN_POINT('Ctrl Pts',(-1.10286118991143,-1.,1.74695004214923));
#23626=CARTESIAN_POINT('Ctrl Pts',(-1.10806728183007,-1.,1.7503286607592));
#23627=CARTESIAN_POINT('Ctrl Pts',(-1.11330807582551,-1.,1.7536777209463));
#23628=CARTESIAN_POINT('Ctrl Pts',(-1.11858293216763,-1.,1.75699720772105));
#23629=CARTESIAN_POINT('Ctrl Pts',(-1.12389096855086,-1.,1.76028671825096));
#23630=CARTESIAN_POINT('Ctrl Pts',(-1.12923123555075,-1.,1.7635457196617));
#23631=CARTESIAN_POINT('Ctrl Pts',(-1.1346029180462,-1.,1.76677384551862));
#23632=CARTESIAN_POINT('Ctrl Pts',(-1.14000548336975,-1.,1.76997111386769));
#23633=CARTESIAN_POINT('Ctrl Pts',(-1.1454385822692,-1.,1.77313777896194));
#23634=CARTESIAN_POINT('Ctrl Pts',(-1.15090197841515,-1.,1.7762742255701));
#23635=CARTESIAN_POINT('Ctrl Pts',(-1.15639547194698,-1.,1.77938085564275));
#23636=CARTESIAN_POINT('Ctrl Pts',(-1.16191881298499,-1.,1.78245795881009));
#23637=CARTESIAN_POINT('Ctrl Pts',(-1.16747166312303,-1.,1.78550566040443));
#23638=CARTESIAN_POINT('Ctrl Pts',(-1.17305363177328,-1.,1.78852398877616));
#23639=CARTESIAN_POINT('Ctrl Pts',(-1.17866429440809,-1.,1.79151291552689));
#23640=CARTESIAN_POINT('Ctrl Pts',(-1.18430321697432,-1.,1.79447240321515));
#23641=CARTESIAN_POINT('Ctrl Pts',(-1.18996997934445,-1.,1.79740245923478));
#23642=CARTESIAN_POINT('Ctrl Pts',(-1.19566418930242,-1.,1.80030314369879));
#23643=CARTESIAN_POINT('Ctrl Pts',(-1.20138548938974,-1.,1.80317454838603));
#23644=CARTESIAN_POINT('Ctrl Pts',(-1.20713356605475,-1.,1.80601678480707));
#23645=CARTESIAN_POINT('Ctrl Pts',(-1.21290815708314,-1.,1.80882996917129));
#23646=CARTESIAN_POINT('Ctrl Pts',(-1.21870906103557,-1.,1.81161420806656));
#23647=CARTESIAN_POINT('Ctrl Pts',(-1.2245361330495,-1.,1.81436959210434));
#23648=CARTESIAN_POINT('Ctrl Pts',(-1.2292186489137,-1.,1.8165508718364));
#23649=CARTESIAN_POINT('Ctrl Pts',(-1.2327422452705,-1.,1.81817389921279));
#23650=CARTESIAN_POINT('Ctrl Pts',(-1.23509651170476,-1.,1.81925017193666));
#23651=CARTESIAN_POINT('Ctrl Pts',(-1.23627494547115,-1.,1.81978687191668));
#23652=CARTESIAN_POINT('',(-1.34869019493419,-1.,1.73811241238545));
#23653=CARTESIAN_POINT('',(-1.23627494547115,-1.,1.81978687191668));
#23654=CARTESIAN_POINT('',(-1.15624053661742,-1.,1.31362392696032));
#23655=CARTESIAN_POINT('Ctrl Pts',(-1.34869019493419,-1.,1.73811241238545));
#23656=CARTESIAN_POINT('Ctrl Pts',(-1.34854391898045,-1.,1.73682580585691));
#23657=CARTESIAN_POINT('Ctrl Pts',(-1.34824783112887,-1.,1.73425417885907));
#23658=CARTESIAN_POINT('Ctrl Pts',(-1.34779309152035,-1.,1.7304014965394));
#23659=CARTESIAN_POINT('Ctrl Pts',(-1.34716554819527,-1.,1.72527410680674));
#23660=CARTESIAN_POINT('Ctrl Pts',(-1.34634568653227,-1.,1.7188807715049));
#23661=CARTESIAN_POINT('Ctrl Pts',(-1.34549029589416,-1.,1.71250340686822));
#23662=CARTESIAN_POINT('Ctrl Pts',(-1.34459924533831,-1.,1.70614212266738));
#23663=CARTESIAN_POINT('Ctrl Pts',(-1.34367237124483,-1.,1.69979707754427));
#23664=CARTESIAN_POINT('Ctrl Pts',(-1.34270948206319,-1.,1.6934684849687));
#23665=CARTESIAN_POINT('Ctrl Pts',(-1.341710374848,-1.,1.68715660868764));
#23666=CARTESIAN_POINT('Ctrl Pts',(-1.34067485185203,-1.,1.68086176030362));
#23667=CARTESIAN_POINT('Ctrl Pts',(-1.3396027347034,-1.,1.67458429426086));
#23668=CARTESIAN_POINT('Ctrl Pts',(-1.33849388654388,-1.,1.66832460783989));
#23669=CARTESIAN_POINT('Ctrl Pts',(-1.33734820885262,-1.,1.66208312541983));
#23670=CARTESIAN_POINT('Ctrl Pts',(-1.33616559745172,-1.,1.65586025952593));
#23671=CARTESIAN_POINT('Ctrl Pts',(-1.33494590467993,-1.,1.6496563728683));
#23672=CARTESIAN_POINT('Ctrl Pts',(-1.33368890676572,-1.,1.6434717485603));
#23673=CARTESIAN_POINT('Ctrl Pts',(-1.33239425103724,-1.,1.63730653475089));
#23674=CARTESIAN_POINT('Ctrl Pts',(-1.33106149345645,-1.,1.63116079730923));
#23675=CARTESIAN_POINT('Ctrl Pts',(-1.3296901950568,-1.,1.62503464209797));
#23676=CARTESIAN_POINT('Ctrl Pts',(-1.32828000610449,-1.,1.61892832270724));
#23677=CARTESIAN_POINT('Ctrl Pts',(-1.32683074483356,-1.,1.6128423401575));
#23678=CARTESIAN_POINT('Ctrl Pts',(-1.32534250785782,-1.,1.60677758290954));
#23679=CARTESIAN_POINT('Ctrl Pts',(-1.32381550858256,-1.,1.60073511858687));
#23680=CARTESIAN_POINT('Ctrl Pts',(-1.32224985747682,-1.,1.59471591079403));
#23681=CARTESIAN_POINT('Ctrl Pts',(-1.32064537110892,-1.,1.58872057258245));
#23682=CARTESIAN_POINT('Ctrl Pts',(-1.31900135021432,-1.,1.58274907898834));
#23683=CARTESIAN_POINT('Ctrl Pts',(-1.31731642317187,-1.,1.5768005650559));
#23684=CARTESIAN_POINT('Ctrl Pts',(-1.31558903860016,-1.,1.57087397835723));
#23685=CARTESIAN_POINT('Ctrl Pts',(-1.31381795281002,-1.,1.56496872402353));
#23686=CARTESIAN_POINT('Ctrl Pts',(-1.31200264341696,-1.,1.55908521254821));
#23687=CARTESIAN_POINT('Ctrl Pts',(-1.31014393684222,-1.,1.55322568759481));
#23688=CARTESIAN_POINT('Ctrl Pts',(-1.30824393907473,-1.,1.54739413957185));
#23689=CARTESIAN_POINT('Ctrl Pts',(-1.30630475189556,-1.,1.54159462645432));
#23690=CARTESIAN_POINT('Ctrl Pts',(-1.30432735639489,-1.,1.53582981268977));
#23691=CARTESIAN_POINT('Ctrl Pts',(-1.30231064395568,-1.,1.53009970283891));
#23692=CARTESIAN_POINT('Ctrl Pts',(-1.30024984366328,-1.,1.52439957861062));
#23693=CARTESIAN_POINT('Ctrl Pts',(-1.29813791800747,-1.,1.51872184912724));
#23694=CARTESIAN_POINT('Ctrl Pts',(-1.29596850710509,-1.,1.51305994241402));
#23695=CARTESIAN_POINT('Ctrl Pts',(-1.29373841372842,-1.,1.50741159078365));
#23696=CARTESIAN_POINT('Ctrl Pts',(-1.29145022885181,-1.,1.50178230149776));
#23697=CARTESIAN_POINT('Ctrl Pts',(-1.28911506584254,-1.,1.49618896881754));
#23698=CARTESIAN_POINT('Ctrl Pts',(-1.2867467611644,-1.,1.4906522831278));
#23699=CARTESIAN_POINT('Ctrl Pts',(-1.28435533880201,-1.,1.4851881711891));
#23700=CARTESIAN_POINT('Ctrl Pts',(-1.28194158939517,-1.,1.47980070347095));
#23701=CARTESIAN_POINT('Ctrl Pts',(-1.2794891824849,-1.,1.4744717526707));
#23702=CARTESIAN_POINT('Ctrl Pts',(-1.27696414831089,-1.,1.46916035917133));
#23703=CARTESIAN_POINT('Ctrl Pts',(-1.27433119897822,-1.,1.46382431332476));
#23704=CARTESIAN_POINT('Ctrl Pts',(-1.27156805265289,-1.,1.45843906294697));
#23705=CARTESIAN_POINT('Ctrl Pts',(-1.2686778680489,-1.,1.45301422764247));
#23706=CARTESIAN_POINT('Ctrl Pts',(-1.26570925118868,-1.,1.44761985001662));
#23707=CARTESIAN_POINT('Ctrl Pts',(-1.26273903323859,-1.,1.44236470511303));
#23708=CARTESIAN_POINT('Ctrl Pts',(-1.25983531012005,-1.,1.43734919180848));
#23709=CARTESIAN_POINT('Ctrl Pts',(-1.25702687965755,-1.,1.43262645609691));
#23710=CARTESIAN_POINT('Ctrl Pts',(-1.25426945222639,-1.,1.42815938799387));
#23711=CARTESIAN_POINT('Ctrl Pts',(-1.2514145557001,-1.,1.42378102115575));
#23712=CARTESIAN_POINT('Ctrl Pts',(-1.24824430986571,-1.,1.41923722596025));
#23713=CARTESIAN_POINT('Ctrl Pts',(-1.24450600513056,-1.,1.41422913175179));
#23714=CARTESIAN_POINT('Ctrl Pts',(-1.23994455029534,-1.,1.40845295531283));
#23715=CARTESIAN_POINT('Ctrl Pts',(-1.23434087290423,-1.,1.40164708206106));
#23716=CARTESIAN_POINT('Ctrl Pts',(-1.22752961899387,-1.,1.39361389568796));
#23717=CARTESIAN_POINT('Ctrl Pts',(-1.21938737280852,-1.,1.38420564527715));
#23718=CARTESIAN_POINT('Ctrl Pts',(-1.20982812925645,-1.,1.37331915607905));
#23719=CARTESIAN_POINT('Ctrl Pts',(-1.1987959077932,-1.,1.36088705043885));
#23720=CARTESIAN_POINT('Ctrl Pts',(-1.18625865667441,-1.,1.34687054001093));
#23721=CARTESIAN_POINT('Ctrl Pts',(-1.17501305789857,-1.,1.33437539347008));
#23722=CARTESIAN_POINT('Ctrl Pts',(-1.16589330093588,-1.,1.32428080721772));
#23723=CARTESIAN_POINT('Ctrl Pts',(-1.15950888730809,-1.,1.31722977216397));
#23724=CARTESIAN_POINT('Ctrl Pts',(-1.15624053661742,-1.,1.31362392696032));
#23725=CARTESIAN_POINT('',(-1.31362392696033,-1.,1.15624053661742));
#23726=CARTESIAN_POINT('Origin',(0.,-1.,0.));
#23727=CARTESIAN_POINT('',(-1.73811241238545,-1.,1.34869019493419));
#23728=CARTESIAN_POINT('Ctrl Pts',(-1.31362392696033,-1.,1.15624053661742));
#23729=CARTESIAN_POINT('Ctrl Pts',(-1.3172297721596,-1.,1.15950888730433));
#23730=CARTESIAN_POINT('Ctrl Pts',(-1.32428080720544,-1.,1.16589330092532));
#23731=CARTESIAN_POINT('Ctrl Pts',(-1.33437539344842,-1.,1.17501305787994));
#23732=CARTESIAN_POINT('Ctrl Pts',(-1.34687053998157,-1.,1.18625865664915));
#23733=CARTESIAN_POINT('Ctrl Pts',(-1.36088705040677,-1.,1.1987959077656));
#23734=CARTESIAN_POINT('Ctrl Pts',(-1.37331915604962,-1.,1.20982812923113));
#23735=CARTESIAN_POINT('Ctrl Pts',(-1.38420564525391,-1.,1.21938737278853));
#23736=CARTESIAN_POINT('Ctrl Pts',(-1.39361389567257,-1.,1.22752961898063));
#23737=CARTESIAN_POINT('Ctrl Pts',(-1.40164708205345,-1.,1.23434087289768));
#23738=CARTESIAN_POINT('Ctrl Pts',(-1.40845295531151,-1.,1.23994455029421));
#23739=CARTESIAN_POINT('Ctrl Pts',(-1.41422913175437,-1.,1.24450600513278));
#23740=CARTESIAN_POINT('Ctrl Pts',(-1.41923722596421,-1.,1.24824430986911));
#23741=CARTESIAN_POINT('Ctrl Pts',(-1.42378102115911,-1.,1.25141455570299));
#23742=CARTESIAN_POINT('Ctrl Pts',(-1.42815938799555,-1.,1.25426945222783));
#23743=CARTESIAN_POINT('Ctrl Pts',(-1.43262645609679,-1.,1.25702687965744));
#23744=CARTESIAN_POINT('Ctrl Pts',(-1.43734919180719,-1.,1.25983531011894));
#23745=CARTESIAN_POINT('Ctrl Pts',(-1.44236470511145,-1.,1.26273903323723));
#23746=CARTESIAN_POINT('Ctrl Pts',(-1.44761985001544,-1.,1.26570925118767));
#23747=CARTESIAN_POINT('Ctrl Pts',(-1.45301422764205,-1.,1.26867786804854));
#23748=CARTESIAN_POINT('Ctrl Pts',(-1.45843906294725,-1.,1.27156805265312));
#23749=CARTESIAN_POINT('Ctrl Pts',(-1.4638243133254,-1.,1.27433119897877));
#23750=CARTESIAN_POINT('Ctrl Pts',(-1.46916035917197,-1.,1.27696414831144));
#23751=CARTESIAN_POINT('Ctrl Pts',(-1.4744717526711,-1.,1.27948918248524));
#23752=CARTESIAN_POINT('Ctrl Pts',(-1.47980070347102,-1.,1.28194158939522));
#23753=CARTESIAN_POINT('Ctrl Pts',(-1.48518817118891,-1.,1.28435533880184));
#23754=CARTESIAN_POINT('Ctrl Pts',(-1.4906522831275,-1.,1.28674676116415));
#23755=CARTESIAN_POINT('Ctrl Pts',(-1.49618896881729,-1.,1.28911506584232));
#23756=CARTESIAN_POINT('Ctrl Pts',(-1.50178230149764,-1.,1.29145022885171));
#23757=CARTESIAN_POINT('Ctrl Pts',(-1.50741159078367,-1.,1.29373841372843));
#23758=CARTESIAN_POINT('Ctrl Pts',(-1.51305994241412,-1.,1.29596850710518));
#23759=CARTESIAN_POINT('Ctrl Pts',(-1.51872184912735,-1.,1.29813791800757));
#23760=CARTESIAN_POINT('Ctrl Pts',(-1.5243995786107,-1.,1.30024984366334));
#23761=CARTESIAN_POINT('Ctrl Pts',(-1.53009970283893,-1.,1.3023106439557));
#23762=CARTESIAN_POINT('Ctrl Pts',(-1.53582981268976,-1.,1.30432735639487));
#23763=CARTESIAN_POINT('Ctrl Pts',(-1.54159462645428,-1.,1.30630475189553));
#23764=CARTESIAN_POINT('Ctrl Pts',(-1.54739413957183,-1.,1.30824393907471));
#23765=CARTESIAN_POINT('Ctrl Pts',(-1.55322568759481,-1.,1.31014393684221));
#23766=CARTESIAN_POINT('Ctrl Pts',(-1.55908521254822,-1.,1.31200264341696));
#23767=CARTESIAN_POINT('Ctrl Pts',(-1.56496872402352,-1.,1.31381795281002));
#23768=CARTESIAN_POINT('Ctrl Pts',(-1.57087397835721,-1.,1.31558903860015));
#23769=CARTESIAN_POINT('Ctrl Pts',(-1.57680056505585,-1.,1.31731642317183));
#23770=CARTESIAN_POINT('Ctrl Pts',(-1.58274907898829,-1.,1.31900135021428));
#23771=CARTESIAN_POINT('Ctrl Pts',(-1.58872057258244,-1.,1.32064537110891));
#23772=CARTESIAN_POINT('Ctrl Pts',(-1.59471591079408,-1.,1.32224985747686));
#23773=CARTESIAN_POINT('Ctrl Pts',(-1.600735118587,-1.,1.32381550858266));
#23774=CARTESIAN_POINT('Ctrl Pts',(-1.6067775829097,-1.,1.32534250785794));
#23775=CARTESIAN_POINT('Ctrl Pts',(-1.61284234015762,-1.,1.32683074483365));
#23776=CARTESIAN_POINT('Ctrl Pts',(-1.61892832270723,-1.,1.32828000610448));
#23777=CARTESIAN_POINT('Ctrl Pts',(-1.62503464209777,-1.,1.32969019505665));
#23778=CARTESIAN_POINT('Ctrl Pts',(-1.63116079730887,-1.,1.33106149345618));
#23779=CARTESIAN_POINT('Ctrl Pts',(-1.6373065347505,-1.,1.33239425103694));
#23780=CARTESIAN_POINT('Ctrl Pts',(-1.64347174856007,-1.,1.33368890676554));
#23781=CARTESIAN_POINT('Ctrl Pts',(-1.64965637286843,-1.,1.33494590468003));
#23782=CARTESIAN_POINT('Ctrl Pts',(-1.65586025952651,-1.,1.33616559745217));
#23783=CARTESIAN_POINT('Ctrl Pts',(-1.66208312542073,-1.,1.33734820885331));
#23784=CARTESIAN_POINT('Ctrl Pts',(-1.66832460784078,-1.,1.33849388654458));
#23785=CARTESIAN_POINT('Ctrl Pts',(-1.67458429426126,-1.,1.33960273470372));
#23786=CARTESIAN_POINT('Ctrl Pts',(-1.68086176030308,-1.,1.3406748518516));
#23787=CARTESIAN_POINT('Ctrl Pts',(-1.68715660868602,-1.,1.34171037484673));
#23788=CARTESIAN_POINT('Ctrl Pts',(-1.6934684849664,-1.,1.34270948206139));
#23789=CARTESIAN_POINT('Ctrl Pts',(-1.69979707754221,-1.,1.34367237124322));
#23790=CARTESIAN_POINT('Ctrl Pts',(-1.70614212266676,-1.,1.34459924533783));
#23791=CARTESIAN_POINT('Ctrl Pts',(-1.71250340687011,-1.,1.34549029589563));
#23792=CARTESIAN_POINT('Ctrl Pts',(-1.7188807715095,-1.,1.34634568653586));
#23793=CARTESIAN_POINT('Ctrl Pts',(-1.72527410681298,-1.,1.34716554820013));
#23794=CARTESIAN_POINT('Ctrl Pts',(-1.73040149654497,-1.,1.3477930915247));
#23795=CARTESIAN_POINT('Ctrl Pts',(-1.73425417886255,-1.,1.34824783113158));
#23796=CARTESIAN_POINT('Ctrl Pts',(-1.73682580585819,-1.,1.34854391898145));
#23797=CARTESIAN_POINT('Ctrl Pts',(-1.73811241238545,-1.,1.34869019493419));
#23798=CARTESIAN_POINT('',(-1.81978687191668,-1.,1.23627494547115));
#23799=CARTESIAN_POINT('',(-1.73811241238545,-1.,1.34869019493419));
#23800=CARTESIAN_POINT('',(-1.5055822144029,-1.,0.892032620296855));
#23801=CARTESIAN_POINT('Ctrl Pts',(-1.81978687191668,-1.,1.23627494547115));
#23802=CARTESIAN_POINT('Ctrl Pts',(-1.81925017193531,-1.,1.23509651170384));
#23803=CARTESIAN_POINT('Ctrl Pts',(-1.81817389920914,-1.,1.23274224526804));
#23804=CARTESIAN_POINT('Ctrl Pts',(-1.81655087183054,-1.,1.22921864890975));
#23805=CARTESIAN_POINT('Ctrl Pts',(-1.81436959209778,-1.,1.22453613304507));
#23806=CARTESIAN_POINT('Ctrl Pts',(-1.81161420806172,-1.,1.2187090610323));
#23807=CARTESIAN_POINT('Ctrl Pts',(-1.80882996916931,-1.,1.2129081570818));
#23808=CARTESIAN_POINT('Ctrl Pts',(-1.80601678480772,-1.,1.20713356605519));
#23809=CARTESIAN_POINT('Ctrl Pts',(-1.8031745483882,-1.,1.2013854893912));
#23810=CARTESIAN_POINT('Ctrl Pts',(-1.80030314370121,-1.,1.19566418930405));
#23811=CARTESIAN_POINT('Ctrl Pts',(-1.79740245923649,-1.,1.1899699793456));
#23812=CARTESIAN_POINT('Ctrl Pts',(-1.79447240321572,-1.,1.18430321697471));
#23813=CARTESIAN_POINT('Ctrl Pts',(-1.79151291552646,-1.,1.17866429440781));
#23814=CARTESIAN_POINT('Ctrl Pts',(-1.78852398877523,-1.,1.17305363177265));
#23815=CARTESIAN_POINT('Ctrl Pts',(-1.78550566040349,-1.,1.16747166312239));
#23816=CARTESIAN_POINT('Ctrl Pts',(-1.78245795880949,-1.,1.16191881298458));
#23817=CARTESIAN_POINT('Ctrl Pts',(-1.77938085564261,-1.,1.15639547194689));
#23818=CARTESIAN_POINT('Ctrl Pts',(-1.77627422557034,-1.,1.15090197841531));
#23819=CARTESIAN_POINT('Ctrl Pts',(-1.77313777896234,-1.,1.14543858226948));
#23820=CARTESIAN_POINT('Ctrl Pts',(-1.76997111386806,-1.,1.14000548337));
#23821=CARTESIAN_POINT('Ctrl Pts',(-1.76677384551883,-1.,1.13460291804635));
#23822=CARTESIAN_POINT('Ctrl Pts',(-1.76354571966171,-1.,1.12923123555076));
#23823=CARTESIAN_POINT('Ctrl Pts',(-1.76028671825084,-1.,1.12389096855078));
#23824=CARTESIAN_POINT('Ctrl Pts',(-1.75699720772089,-1.,1.11858293216752));
#23825=CARTESIAN_POINT('Ctrl Pts',(-1.75367772094617,-1.,1.11330807582542));
#23826=CARTESIAN_POINT('Ctrl Pts',(-1.75032866075914,-1.,1.10806728183003));
#23827=CARTESIAN_POINT('Ctrl Pts',(-1.74695004214924,-1.,1.10286118991144));
#23828=CARTESIAN_POINT('Ctrl Pts',(-1.74354119236212,-1.,1.09768999241229));
#23829=CARTESIAN_POINT('Ctrl Pts',(-1.74010053962252,-1.,1.09255329056496));
#23830=CARTESIAN_POINT('Ctrl Pts',(-1.73662628326093,-1.,1.08745056285429));
#23831=CARTESIAN_POINT('Ctrl Pts',(-1.73311705663407,-1.,1.08238162784749));
#23832=CARTESIAN_POINT('Ctrl Pts',(-1.72957248977424,-1.,1.0773470373727));
#23833=CARTESIAN_POINT('Ctrl Pts',(-1.72599406198489,-1.,1.07234866990252));
#23834=CARTESIAN_POINT('Ctrl Pts',(-1.72238500928456,-1.,1.06738966975463));
#23835=CARTESIAN_POINT('Ctrl Pts',(-1.71874858456908,-1.,1.0624732468065));
#23836=CARTESIAN_POINT('Ctrl Pts',(-1.71508654427022,-1.,1.05760163192481));
#23837=CARTESIAN_POINT('Ctrl Pts',(-1.71139783543986,-1.,1.05277517202854));
#23838=CARTESIAN_POINT('Ctrl Pts',(-1.70767646263641,-1.,1.0479908540499));
#23839=CARTESIAN_POINT('Ctrl Pts',(-1.70391338707969,-1.,1.04324363334546));
#23840=CARTESIAN_POINT('Ctrl Pts',(-1.70010052930951,-1.,1.03852922490782));
#23841=CARTESIAN_POINT('Ctrl Pts',(-1.69623414782769,-1.,1.03384646003587));
#23842=CARTESIAN_POINT('Ctrl Pts',(-1.69231840863471,-1.,1.02919977579155));
#23843=CARTESIAN_POINT('Ctrl Pts',(-1.68836910178475,-1.,1.02460180535272));
#23844=CARTESIAN_POINT('Ctrl Pts',(-1.68440578021739,-1.,1.02006795074222));
#23845=CARTESIAN_POINT('Ctrl Pts',(-1.6804428989482,-1.,1.01561026162787));
#23846=CARTESIAN_POINT('Ctrl Pts',(-1.67648246776457,-1.,1.01123236493507));
#23847=CARTESIAN_POINT('Ctrl Pts',(-1.67250335383248,-1.,1.00692206696387));
#23848=CARTESIAN_POINT('Ctrl Pts',(-1.66846059277231,-1.,1.00265091003682));
#23849=CARTESIAN_POINT('Ctrl Pts',(-1.66430758030304,-1.,0.998389654952317));
#23850=CARTESIAN_POINT('Ctrl Pts',(-1.66001553809916,-1.,0.994121836661116));
#23851=CARTESIAN_POINT('Ctrl Pts',(-1.65559044289746,-1.,0.98985562785445));
#23852=CARTESIAN_POINT('Ctrl Pts',(-1.6511001661277,-1.,0.985642622921626));
#23853=CARTESIAN_POINT('Ctrl Pts',(-1.64665139190834,-1.,0.981562530940574));
#23854=CARTESIAN_POINT('Ctrl Pts',(-1.64233990826831,-1.,0.977689794120297));
#23855=CARTESIAN_POINT('Ctrl Pts',(-1.63820952658157,-1.,0.974066058287501));
#23856=CARTESIAN_POINT('Ctrl Pts',(-1.63420665729609,-1.,0.970669715996356));
#23857=CARTESIAN_POINT('Ctrl Pts',(-1.63013849959083,-1.,0.967387853228041));
#23858=CARTESIAN_POINT('Ctrl Pts',(-1.6257193066974,-1.,0.964046107037821));
#23859=CARTESIAN_POINT('Ctrl Pts',(-1.62061638139929,-1.,0.960438326099958));
#23860=CARTESIAN_POINT('Ctrl Pts',(-1.61449324337233,-1.,0.956354422921573));
#23861=CARTESIAN_POINT('Ctrl Pts',(-1.60706069897794,-1.,0.951613284361248));
#23862=CARTESIAN_POINT('Ctrl Pts',(-1.59810042045408,-1.,0.946078063325796));
#23863=CARTESIAN_POINT('Ctrl Pts',(-1.58744937489796,-1.,0.939646377909319));
#23864=CARTESIAN_POINT('Ctrl Pts',(-1.57499388385561,-1.,0.932246680128849));
#23865=CARTESIAN_POINT('Ctrl Pts',(-1.56065988582509,-1.,0.923832188966322));
#23866=CARTESIAN_POINT('Ctrl Pts',(-1.54440491152808,-1.,0.91437591904658));
#23867=CARTESIAN_POINT('Ctrl Pts',(-1.52984849890434,-1.,0.905967409640499));
#23868=CARTESIAN_POINT('Ctrl Pts',(-1.51805569591479,-1.,0.89918504749193));
#23869=CARTESIAN_POINT('Ctrl Pts',(-1.50980486807181,-1.,0.894452006967538));
#23870=CARTESIAN_POINT('Ctrl Pts',(-1.5055822144029,-1.,0.892032620296855));
#23871=CARTESIAN_POINT('',(-1.60662857109684,-1.,0.693717979106305));
#23872=CARTESIAN_POINT('Origin',(0.,-1.,0.));
#23873=CARTESIAN_POINT('',(-2.0698113262342,-1.,0.7455743247944));
#23874=CARTESIAN_POINT('Ctrl Pts',(-1.60662857109684,-1.,0.693717979106305));
#23875=CARTESIAN_POINT('Ctrl Pts',(-1.61106790957619,-1.,0.69571209787897));
#23876=CARTESIAN_POINT('Ctrl Pts',(-1.61974673471117,-1.,0.699605146398837));
#23877=CARTESIAN_POINT('Ctrl Pts',(-1.6321654166204,-1.,0.705159151977294));
#23878=CARTESIAN_POINT('Ctrl Pts',(-1.64752408828442,-1.,0.711993139340447));
#23879=CARTESIAN_POINT('Ctrl Pts',(-1.66472880551777,-1.,0.71958543378795));
#23880=CARTESIAN_POINT('Ctrl Pts',(-1.67996158451922,-1.,0.726235967982445));
#23881=CARTESIAN_POINT('Ctrl Pts',(-1.69326921972915,-1.,0.731963238685357));
#23882=CARTESIAN_POINT('Ctrl Pts',(-1.70473309004249,-1.,0.736799665716932));
#23883=CARTESIAN_POINT('Ctrl Pts',(-1.71447789751001,-1.,0.74079516202821));
#23884=CARTESIAN_POINT('Ctrl Pts',(-1.72268229916769,-1.,0.744021445433093));
#23885=CARTESIAN_POINT('Ctrl Pts',(-1.72958533647714,-1.,0.746574710097752));
#23886=CARTESIAN_POINT('Ctrl Pts',(-1.7355035168033,-1.,0.74858246295687));
#23887=CARTESIAN_POINT('Ctrl Pts',(-1.74080458267114,-1.,0.750193435981249));
#23888=CARTESIAN_POINT('Ctrl Pts',(-1.74585086852502,-1.,0.751555614164482));
#23889=CARTESIAN_POINT('Ctrl Pts',(-1.75095139468794,-1.,0.752797683531314));
#23890=CARTESIAN_POINT('Ctrl Pts',(-1.75631083600019,-1.,0.754009254027829));
#23891=CARTESIAN_POINT('Ctrl Pts',(-1.76197817240128,-1.,0.755220979974461));
#23892=CARTESIAN_POINT('Ctrl Pts',(-1.76789396002998,-1.,0.75642189602781));
#23893=CARTESIAN_POINT('Ctrl Pts',(-1.77394167108292,-1.,0.757578264077029));
#23894=CARTESIAN_POINT('Ctrl Pts',(-1.77999411220945,-1.,0.758650626677518));
#23895=CARTESIAN_POINT('Ctrl Pts',(-1.78596964884604,-1.,0.759614401110189));
#23896=CARTESIAN_POINT('Ctrl Pts',(-1.7918581561088,-1.,0.760469555880749));
#23897=CARTESIAN_POINT('Ctrl Pts',(-1.79768986997783,-1.,0.761229695230558));
#23898=CARTESIAN_POINT('Ctrl Pts',(-1.80351583877342,-1.,0.761915336443547));
#23899=CARTESIAN_POINT('Ctrl Pts',(-1.80938551463965,-1.,0.762546129463938));
#23900=CARTESIAN_POINT('Ctrl Pts',(-1.8153211840553,-1.,0.763132003836634));
#23901=CARTESIAN_POINT('Ctrl Pts',(-1.82131873145266,-1.,0.763673465462726));
#23902=CARTESIAN_POINT('Ctrl Pts',(-1.82735991200065,-1.,0.764165902605995));
#23903=CARTESIAN_POINT('Ctrl Pts',(-1.83342077227142,-1.,0.764602549687853));
#23904=CARTESIAN_POINT('Ctrl Pts',(-1.83948181064835,-1.,0.764978057881737));
#23905=CARTESIAN_POINT('Ctrl Pts',(-1.84553698875924,-1.,0.765291664862029));
#23906=CARTESIAN_POINT('Ctrl Pts',(-1.85158945130063,-1.,0.765545710619062));
#23907=CARTESIAN_POINT('Ctrl Pts',(-1.85764741390394,-1.,0.765744212909318));
#23908=CARTESIAN_POINT('Ctrl Pts',(-1.86372027063312,-1.,0.765891519092547));
#23909=CARTESIAN_POINT('Ctrl Pts',(-1.86981398314341,-1.,0.765990708546091));
#23910=CARTESIAN_POINT('Ctrl Pts',(-1.87592888967883,-1.,0.766042837036744));
#23911=CARTESIAN_POINT('Ctrl Pts',(-1.88206215302561,-1.,0.766047794851864));
#23912=CARTESIAN_POINT('Ctrl Pts',(-1.88820926433409,-1.,0.766004837062091));
#23913=CARTESIAN_POINT('Ctrl Pts',(-1.89436577771388,-1.,0.765913193856978));
#23914=CARTESIAN_POINT('Ctrl Pts',(-1.90052930393596,-1.,0.765772772593386));
#23915=CARTESIAN_POINT('Ctrl Pts',(-1.90669961402356,-1.,0.765584196937919));
#23916=CARTESIAN_POINT('Ctrl Pts',(-1.91287765805169,-1.,0.765348465884722));
#23917=CARTESIAN_POINT('Ctrl Pts',(-1.91906491634196,-1.,0.765066729667088));
#23918=CARTESIAN_POINT('Ctrl Pts',(-1.92526263537048,-1.,0.764740025488211));
#23919=CARTESIAN_POINT('Ctrl Pts',(-1.93147105496382,-1.,0.76436901067394));
#23920=CARTESIAN_POINT('Ctrl Pts',(-1.93768964875886,-1.,0.763954049121458));
#23921=CARTESIAN_POINT('Ctrl Pts',(-1.9439174661764,-1.,0.763495333538629));
#23922=CARTESIAN_POINT('Ctrl Pts',(-1.95015342590024,-1.,0.762992990878769));
#23923=CARTESIAN_POINT('Ctrl Pts',(-1.95639665309869,-1.,0.762447203806179));
#23924=CARTESIAN_POINT('Ctrl Pts',(-1.96264672744186,-1.,0.761858300014423));
#23925=CARTESIAN_POINT('Ctrl Pts',(-1.96890351582499,-1.,0.76122669048382));
#23926=CARTESIAN_POINT('Ctrl Pts',(-1.97516705321494,-1.,0.760552825409757));
#23927=CARTESIAN_POINT('Ctrl Pts',(-1.98143741418172,-1.,0.75983714745219));
#23928=CARTESIAN_POINT('Ctrl Pts',(-1.98771456680874,-1.,0.759080037802488));
#23929=CARTESIAN_POINT('Ctrl Pts',(-1.99399831098817,-1.,0.758281796766761));
#23930=CARTESIAN_POINT('Ctrl Pts',(-2.00028834739178,-1.,0.757442676862724));
#23931=CARTESIAN_POINT('Ctrl Pts',(-2.0065843158773,-1.,0.75656290464667));
#23932=CARTESIAN_POINT('Ctrl Pts',(-2.01288584328084,-1.,0.755642704957865));
#23933=CARTESIAN_POINT('Ctrl Pts',(-2.01919259405809,-1.,0.754682330722816));
#23934=CARTESIAN_POINT('Ctrl Pts',(-2.02550428623313,-1.,0.753682061112768));
#23935=CARTESIAN_POINT('Ctrl Pts',(-2.03182068456221,-1.,0.752642180487211));
#23936=CARTESIAN_POINT('Ctrl Pts',(-2.03814160092099,-1.,0.751562963361115));
#23937=CARTESIAN_POINT('Ctrl Pts',(-2.04446689147979,-1.,0.750444657875576));
#23938=CARTESIAN_POINT('Ctrl Pts',(-2.05079645592154,-1.,0.749287468665046));
#23939=CARTESIAN_POINT('Ctrl Pts',(-2.05713023031006,-1.,0.748091554183802));
#23940=CARTESIAN_POINT('Ctrl Pts',(-2.06220058927826,-1.,0.747103932787919));
#23941=CARTESIAN_POINT('Ctrl Pts',(-2.06600523016815,-1.,0.7463458715442));
#23942=CARTESIAN_POINT('Ctrl Pts',(-2.06854248895728,-1.,0.745832791378367));
#23943=CARTESIAN_POINT('Ctrl Pts',(-2.0698113262342,-1.,0.7455743247944));
#23944=CARTESIAN_POINT('',(-2.11275013067528,-1.,0.61342227326009));
#23945=CARTESIAN_POINT('',(-2.0698113262342,-1.,0.7455743247944));
#23946=CARTESIAN_POINT('',(-1.7075470150345,-1.,0.383122945602004));
#23947=CARTESIAN_POINT('Ctrl Pts',(-2.11275013067528,-1.,0.61342227326009));
#23948=CARTESIAN_POINT('Ctrl Pts',(-2.11187554259986,-1.,0.6124673655618));
#23949=CARTESIAN_POINT('Ctrl Pts',(-2.11012443807238,-1.,0.610560911689899));
#23950=CARTESIAN_POINT('Ctrl Pts',(-2.1074919961518,-1.,0.607711315454876));
#23951=CARTESIAN_POINT('Ctrl Pts',(-2.10397049886949,-1.,0.60393203073603));
#23952=CARTESIAN_POINT('Ctrl Pts',(-2.0995493086477,-1.,0.599241616420533));
#23953=CARTESIAN_POINT('Ctrl Pts',(-2.0951087622027,-1.,0.594585006052162));
#23954=CARTESIAN_POINT('Ctrl Pts',(-2.09064881812129,-1.,0.589962365403406));
#23955=CARTESIAN_POINT('Ctrl Pts',(-2.08616943727951,-1.,0.585373918991617));
#23956=CARTESIAN_POINT('Ctrl Pts',(-2.08167059018418,-1.,0.580819952108063));
#23957=CARTESIAN_POINT('Ctrl Pts',(-2.07715226767559,-1.,0.576300797416844));
#23958=CARTESIAN_POINT('Ctrl Pts',(-2.07261449292824,-1.,0.571816823242603));
#23959=CARTESIAN_POINT('Ctrl Pts',(-2.06805732997334,-1.,0.567368421181087));
#23960=CARTESIAN_POINT('Ctrl Pts',(-2.06348090160589,-1.,0.562955993082261));
#23961=CARTESIAN_POINT('Ctrl Pts',(-2.05888537756462,-1.,0.558579940185151));
#23962=CARTESIAN_POINT('Ctrl Pts',(-2.05427091604413,-1.,0.554240657463906));
#23963=CARTESIAN_POINT('Ctrl Pts',(-2.04963761077958,-1.,0.549938525150295));
#23964=CARTESIAN_POINT('Ctrl Pts',(-2.04498544714588,-1.,0.54567390381743));
#23965=CARTESIAN_POINT('Ctrl Pts',(-2.04031422690527,-1.,0.541447120615659));
#23966=CARTESIAN_POINT('Ctrl Pts',(-2.03562362954037,-1.,0.537258489833262));
#23967=CARTESIAN_POINT('Ctrl Pts',(-2.03091336214426,-1.,0.533108355132976));
#23968=CARTESIAN_POINT('Ctrl Pts',(-2.0261832908329,-1.,0.528997127241914));
#23969=CARTESIAN_POINT('Ctrl Pts',(-2.02143356304698,-1.,0.524925318333476));
#23970=CARTESIAN_POINT('Ctrl Pts',(-2.01666477917286,-1.,0.52089359039937));
#23971=CARTESIAN_POINT('Ctrl Pts',(-2.01187773939242,-1.,0.516902681728687));
#23972=CARTESIAN_POINT('Ctrl Pts',(-2.00707309946949,-1.,0.512953306961792));
#23973=CARTESIAN_POINT('Ctrl Pts',(-2.00225107134734,-1.,0.509046069886157));
#23974=CARTESIAN_POINT('Ctrl Pts',(-1.99741107463572,-1.,0.505181361323026));
#23975=CARTESIAN_POINT('Ctrl Pts',(-1.99255149126155,-1.,0.501359287727146));
#23976=CARTESIAN_POINT('Ctrl Pts',(-1.98767044752932,-1.,0.497579909545574));
#23977=CARTESIAN_POINT('Ctrl Pts',(-1.98276658761821,-1.,0.493843476541494));
#23978=CARTESIAN_POINT('Ctrl Pts',(-1.97783973019229,-1.,0.490150627860952));
#23979=CARTESIAN_POINT('Ctrl Pts',(-1.97289186263272,-1.,0.486502692907659));
#23980=CARTESIAN_POINT('Ctrl Pts',(-1.96792703422362,-1.,0.48290166212069));
#23981=CARTESIAN_POINT('Ctrl Pts',(-1.96294933055943,-1.,0.479349583074855));
#23982=CARTESIAN_POINT('Ctrl Pts',(-1.95796111148177,-1.,0.475848034683176));
#23983=CARTESIAN_POINT('Ctrl Pts',(-1.95296148278133,-1.,0.472397672264072));
#23984=CARTESIAN_POINT('Ctrl Pts',(-1.94794381136514,-1.,0.468997482913135));
#23985=CARTESIAN_POINT('Ctrl Pts',(-1.9428979419619,-1.,0.46564546202603));
#23986=CARTESIAN_POINT('Ctrl Pts',(-1.93781486640821,-1.,0.462340031009056));
#23987=CARTESIAN_POINT('Ctrl Pts',(-1.93269066517934,-1.,0.459081234547926));
#23988=CARTESIAN_POINT('Ctrl Pts',(-1.92753067150476,-1.,0.455872005174371));
#23989=CARTESIAN_POINT('Ctrl Pts',(-1.92235380648502,-1.,0.452719478359432));
#23990=CARTESIAN_POINT('Ctrl Pts',(-1.91718342555755,-1.,0.449632260106662));
#23991=CARTESIAN_POINT('Ctrl Pts',(-1.9120369998112,-1.,0.446617343485711));
#23992=CARTESIAN_POINT('Ctrl Pts',(-1.90691756144898,-1.,0.44367755684915));
#23993=CARTESIAN_POINT('Ctrl Pts',(-1.90180124389086,-1.,0.440807833704038));
#23994=CARTESIAN_POINT('Ctrl Pts',(-1.89663648956466,-1.,0.437995003948244));
#23995=CARTESIAN_POINT('Ctrl Pts',(-1.89136993975504,-1.,0.435225660963383));
#23996=CARTESIAN_POINT('Ctrl Pts',(-1.88596913666793,-1.,0.432493038548748));
#23997=CARTESIAN_POINT('Ctrl Pts',(-1.88044229001832,-1.,0.429803062482344));
#23998=CARTESIAN_POINT('Ctrl Pts',(-1.87486989291484,-1.,0.427183828519102));
#23999=CARTESIAN_POINT('Ctrl Pts',(-1.86937803944323,-1.,0.424678177291359));
#24000=CARTESIAN_POINT('Ctrl Pts',(-1.86408083334028,-1.,0.422327307418275));
#24001=CARTESIAN_POINT('Ctrl Pts',(-1.85903281096686,-1.,0.420157287975619));
#24002=CARTESIAN_POINT('Ctrl Pts',(-1.85417632856234,-1.,0.418164129143534));
#24003=CARTESIAN_POINT('Ctrl Pts',(-1.84929312929882,-1.,0.416300022038864));
#24004=CARTESIAN_POINT('Ctrl Pts',(-1.8440575707371,-1.,0.41448743825434));
#24005=CARTESIAN_POINT('Ctrl Pts',(-1.83808953475839,-1.,0.412633125322161));
#24006=CARTESIAN_POINT('Ctrl Pts',(-1.83100408895216,-1.,0.410641256301675));
#24007=CARTESIAN_POINT('Ctrl Pts',(-1.8224702267854,-1.,0.408428948108533));
#24008=CARTESIAN_POINT('Ctrl Pts',(-1.81223801813988,-1.,0.405933518411838));
#24009=CARTESIAN_POINT('Ctrl Pts',(-1.80012077176221,-1.,0.403107976170441));
#24010=CARTESIAN_POINT('Ctrl Pts',(-1.78598826347533,-1.,0.39991940378308));
#24011=CARTESIAN_POINT('Ctrl Pts',(-1.7697556004756,-1.,0.39634619612042));
#24012=CARTESIAN_POINT('Ctrl Pts',(-1.75137405313962,-1.,0.392375812294307));
#24013=CARTESIAN_POINT('Ctrl Pts',(-1.7349317097561,-1.,0.388877023509191));
#24014=CARTESIAN_POINT('Ctrl Pts',(-1.72162022246158,-1.,0.38607079032701));
#24015=CARTESIAN_POINT('Ctrl Pts',(-1.71231062891958,-1.,0.384119047315542));
#24016=CARTESIAN_POINT('Ctrl Pts',(-1.7075470150345,-1.,0.383122945602004));
#24017=CARTESIAN_POINT('',(-1.74236521665491,-1.,0.163289472382896));
#24018=CARTESIAN_POINT('Origin',(0.,-1.,0.));
#24019=CARTESIAN_POINT('',(-2.19890268624765,-1.,0.069476445021958));
#24020=CARTESIAN_POINT('Ctrl Pts',(-1.74236521665491,-1.,0.163289472382896));
#24021=CARTESIAN_POINT('Ctrl Pts',(-1.7472034950333,-1.,0.163814161002002));
#24022=CARTESIAN_POINT('Ctrl Pts',(-1.75666056638427,-1.,0.164834765707158));
#24023=CARTESIAN_POINT('Ctrl Pts',(-1.77018771684844,-1.,0.1662793551464));
#24024=CARTESIAN_POINT('Ctrl Pts',(-1.7869064998507,-1.,0.168032772805197));
#24025=CARTESIAN_POINT('Ctrl Pts',(-1.80561530629706,-1.,0.169936923904608));
#24026=CARTESIAN_POINT('Ctrl Pts',(-1.82215766811545,-1.,0.171554770204119));
#24027=CARTESIAN_POINT('Ctrl Pts',(-1.83658380527692,-1.,0.1728894428919));
#24028=CARTESIAN_POINT('Ctrl Pts',(-1.8489811319852,-1.,0.173946627587731));
#24029=CARTESIAN_POINT('Ctrl Pts',(-1.85948367088837,-1.,0.17473525927603));
#24030=CARTESIAN_POINT('Ctrl Pts',(-1.86828349694799,-1.,0.175268337590758));
#24031=CARTESIAN_POINT('Ctrl Pts',(-1.87563767773588,-1.,0.175563480746485));
#24032=CARTESIAN_POINT('Ctrl Pts',(-1.88188663145367,-1.,0.175644148889698));
#24033=CARTESIAN_POINT('Ctrl Pts',(-1.88742606273259,-1.,0.175538155840648));
#24034=CARTESIAN_POINT('Ctrl Pts',(-1.892646301985,-1.,0.175274276190844));
#24035=CARTESIAN_POINT('Ctrl Pts',(-1.89788101117132,-1.,0.174879405091263));
#24036=CARTESIAN_POINT('Ctrl Pts',(-1.90335253862834,-1.,0.174375518661085));
#24037=CARTESIAN_POINT('Ctrl Pts',(-1.90911693975267,-1.,0.173776635257817));
#24038=CARTESIAN_POINT('Ctrl Pts',(-1.91511429159527,-1.,0.173090695383496));
#24039=CARTESIAN_POINT('Ctrl Pts',(-1.9212233439798,-1.,0.172321621259514));
#24040=CARTESIAN_POINT('Ctrl Pts',(-1.92731093582036,-1.,0.171471191532988));
#24041=CARTESIAN_POINT('Ctrl Pts',(-1.93329183155539,-1.,0.170541253116201));
#24042=CARTESIAN_POINT('Ctrl Pts',(-1.93915639211581,-1.,0.169534904817491));
#24043=CARTESIAN_POINT('Ctrl Pts',(-1.94493757756931,-1.,0.168455741607556));
#24044=CARTESIAN_POINT('Ctrl Pts',(-1.95069027794294,-1.,0.167307501784475));
#24045=CARTESIAN_POINT('Ctrl Pts',(-1.9564675971873,-1.,0.166093592002812));
#24046=CARTESIAN_POINT('Ctrl Pts',(-1.96229379940136,-1.,0.164816568920269));
#24047=CARTESIAN_POINT('Ctrl Pts',(-1.96816512677967,-1.,0.163478185457734));
#24048=CARTESIAN_POINT('Ctrl Pts',(-1.97406280235188,-1.,0.162079693556288));
#24049=CARTESIAN_POINT('Ctrl Pts',(-1.97996195437559,-1.,0.160622060784611));
#24050=CARTESIAN_POINT('Ctrl Pts',(-1.98584238283292,-1.,0.159106226437299));
#24051=CARTESIAN_POINT('Ctrl Pts',(-1.99169810931908,-1.,0.157533331459227));
#24052=CARTESIAN_POINT('Ctrl Pts',(-1.99753284771497,-1.,0.155904629548783));
#24053=CARTESIAN_POINT('Ctrl Pts',(-2.00335565310543,-1.,0.154221403049722));
#24054=CARTESIAN_POINT('Ctrl Pts',(-2.00917680318424,-1.,0.15248488362145));
#24055=CARTESIAN_POINT('Ctrl Pts',(-2.01500291940238,-1.,0.150696157673078));
#24056=CARTESIAN_POINT('Ctrl Pts',(-2.02083464969894,-1.,0.148856124775337));
#24057=CARTESIAN_POINT('Ctrl Pts',(-2.02666926182017,-1.,0.146965557332583));
#24058=CARTESIAN_POINT('Ctrl Pts',(-2.03250223739942,-1.,0.145025140186057));
#24059=CARTESIAN_POINT('Ctrl Pts',(-2.03832911025912,-1.,0.143035515058209));
#24060=CARTESIAN_POINT('Ctrl Pts',(-2.04414757947916,-1.,0.140997332152546));
#24061=CARTESIAN_POINT('Ctrl Pts',(-2.04995762001328,-1.,0.138911255368966));
#24062=CARTESIAN_POINT('Ctrl Pts',(-2.05576044414264,-1.,0.136777941218043));
#24063=CARTESIAN_POINT('Ctrl Pts',(-2.06155781517842,-1.,0.134598026192106));
#24064=CARTESIAN_POINT('Ctrl Pts',(-2.06735123910326,-1.,0.13237211154771));
#24065=CARTESIAN_POINT('Ctrl Pts',(-2.07314114713063,-1.,0.130100748328403));
#24066=CARTESIAN_POINT('Ctrl Pts',(-2.07892715110987,-1.,0.12778444527612));
#24067=CARTESIAN_POINT('Ctrl Pts',(-2.08470840653643,-1.,0.125423679412061));
#24068=CARTESIAN_POINT('Ctrl Pts',(-2.09048392424825,-1.,0.123018905621083));
#24069=CARTESIAN_POINT('Ctrl Pts',(-2.0962529286773,-1.,0.120570567965122));
#24070=CARTESIAN_POINT('Ctrl Pts',(-2.102015121329,-1.,0.118079107988355));
#24071=CARTESIAN_POINT('Ctrl Pts',(-2.10777050261309,-1.,0.115544957687926));
#24072=CARTESIAN_POINT('Ctrl Pts',(-2.11351924490306,-1.,0.112968534419737));
#24073=CARTESIAN_POINT('Ctrl Pts',(-2.11926155590865,-1.,0.110350236135025));
#24074=CARTESIAN_POINT('Ctrl Pts',(-2.12499752307,-1.,0.10769043523109));
#24075=CARTESIAN_POINT('Ctrl Pts',(-2.13072704887293,-1.,0.104989479152739));
#24076=CARTESIAN_POINT('Ctrl Pts',(-2.13644992667165,-1.,0.1022477005561));
#24077=CARTESIAN_POINT('Ctrl Pts',(-2.14216588396025,-1.,0.0994654261990914));
#24078=CARTESIAN_POINT('Ctrl Pts',(-2.14787463531795,-1.,0.0966429852305457));
#24079=CARTESIAN_POINT('Ctrl Pts',(-2.1535759397817,-1.,0.0937807218867642));
#24080=CARTESIAN_POINT('Ctrl Pts',(-2.15926961544516,-1.,0.0908789888107264));
#24081=CARTESIAN_POINT('Ctrl Pts',(-2.16495552645014,-1.,0.0879381291386921));
#24082=CARTESIAN_POINT('Ctrl Pts',(-2.17063357870952,-1.,0.0849584620835371));
#24083=CARTESIAN_POINT('Ctrl Pts',(-2.176303712113,-1.,0.0819402680872764));
#24084=CARTESIAN_POINT('Ctrl Pts',(-2.18196589448887,-1.,0.0788837727685241));
#24085=CARTESIAN_POINT('Ctrl Pts',(-2.1876201139953,-1.,0.0757891465836146));
#24086=CARTESIAN_POINT('Ctrl Pts',(-2.19213712013662,-1.,0.0732830357306724));
#24087=CARTESIAN_POINT('Ctrl Pts',(-2.19552129484002,-1.,0.0713863779526153));
#24088=CARTESIAN_POINT('Ctrl Pts',(-2.19777582085423,-1.,0.0701143536325489));
#24089=CARTESIAN_POINT('Ctrl Pts',(-2.19890268624765,-1.,0.069476445021958));
#24090=CARTESIAN_POINT('',(-2.19890268624765,-1.,-0.0694764450219585));
#24091=CARTESIAN_POINT('',(-2.19890268624765,-1.,0.069476445021958));
#24092=CARTESIAN_POINT('',(-1.74236521665491,-1.,-0.163289472382896));
#24093=CARTESIAN_POINT('Ctrl Pts',(-2.19890268624765,-1.,-0.0694764450219585));
#24094=CARTESIAN_POINT('Ctrl Pts',(-2.19777582085261,-1.,-0.0701143536324927));
#24095=CARTESIAN_POINT('Ctrl Pts',(-2.19552129483562,-1.,-0.0713863779524629));
#24096=CARTESIAN_POINT('Ctrl Pts',(-2.19213712012956,-1.,-0.0732830357304277));
#24097=CARTESIAN_POINT('Ctrl Pts',(-2.1876201139874,-1.,-0.0757891465833413));
#24098=CARTESIAN_POINT('Ctrl Pts',(-2.18196589448304,-1.,-0.0788837727683229));
#24099=CARTESIAN_POINT('Ctrl Pts',(-2.1763037121106,-1.,-0.0819402680871941));
#24100=CARTESIAN_POINT('Ctrl Pts',(-2.17063357871031,-1.,-0.0849584620835644));
#24101=CARTESIAN_POINT('Ctrl Pts',(-2.16495552645275,-1.,-0.0879381291387824));
#24102=CARTESIAN_POINT('Ctrl Pts',(-2.15926961544808,-1.,-0.0908789888108267));
#24103=CARTESIAN_POINT('Ctrl Pts',(-2.15357593978377,-1.,-0.0937807218868346));
#24104=CARTESIAN_POINT('Ctrl Pts',(-2.14787463531864,-1.,-0.096642985230569));
#24105=CARTESIAN_POINT('Ctrl Pts',(-2.14216588395974,-1.,-0.0994654261990744));
#24106=CARTESIAN_POINT('Ctrl Pts',(-2.13644992667052,-1.,-0.102247700556064));
#24107=CARTESIAN_POINT('Ctrl Pts',(-2.1307270488718,-1.,-0.104989479152703));
#24108=CARTESIAN_POINT('Ctrl Pts',(-2.12499752306927,-1.,-0.107690435231068));
#24109=CARTESIAN_POINT('Ctrl Pts',(-2.11926155590849,-1.,-0.11035023613502));
#24110=CARTESIAN_POINT('Ctrl Pts',(-2.11351924490335,-1.,-0.112968534419746));
#24111=CARTESIAN_POINT('Ctrl Pts',(-2.10777050261359,-1.,-0.11554495768794));
#24112=CARTESIAN_POINT('Ctrl Pts',(-2.10201512132945,-1.,-0.118079107988368));
#24113=CARTESIAN_POINT('Ctrl Pts',(-2.09625292867756,-1.,-0.120570567965129));
#24114=CARTESIAN_POINT('Ctrl Pts',(-2.09048392424826,-1.,-0.123018905621083));
#24115=CARTESIAN_POINT('Ctrl Pts',(-2.08470840653628,-1.,-0.125423679412058));
#24116=CARTESIAN_POINT('Ctrl Pts',(-2.07892715110967,-1.,-0.127784445276116));
#24117=CARTESIAN_POINT('Ctrl Pts',(-2.07314114713047,-1.,-0.130100748328401));
#24118=CARTESIAN_POINT('Ctrl Pts',(-2.06735123910319,-1.,-0.13237211154771));
#24119=CARTESIAN_POINT('Ctrl Pts',(-2.06155781517844,-1.,-0.134598026192107));
#24120=CARTESIAN_POINT('Ctrl Pts',(-2.0557604441427,-1.,-0.136777941218044));
#24121=CARTESIAN_POINT('Ctrl Pts',(-2.04995762001333,-1.,-0.138911255368966));
#24122=CARTESIAN_POINT('Ctrl Pts',(-2.04414757947919,-1.,-0.140997332152545));
#24123=CARTESIAN_POINT('Ctrl Pts',(-2.03832911025913,-1.,-0.143035515058208));
#24124=CARTESIAN_POINT('Ctrl Pts',(-2.03250223739941,-1.,-0.145025140186058));
#24125=CARTESIAN_POINT('Ctrl Pts',(-2.02666926182017,-1.,-0.146965557332586));
#24126=CARTESIAN_POINT('Ctrl Pts',(-2.02083464969897,-1.,-0.148856124775343));
#24127=CARTESIAN_POINT('Ctrl Pts',(-2.01500291940243,-1.,-0.150696157673084));
#24128=CARTESIAN_POINT('Ctrl Pts',(-2.00917680318426,-1.,-0.152484883621452));
#24129=CARTESIAN_POINT('Ctrl Pts',(-2.00335565310539,-1.,-0.154221403049719));
#24130=CARTESIAN_POINT('Ctrl Pts',(-1.99753284771487,-1.,-0.155904629548775));
#24131=CARTESIAN_POINT('Ctrl Pts',(-1.99169810931893,-1.,-0.157533331459215));
#24132=CARTESIAN_POINT('Ctrl Pts',(-1.98584238283279,-1.,-0.159106226437289));
#24133=CARTESIAN_POINT('Ctrl Pts',(-1.97996195437557,-1.,-0.16062206078461));
#24134=CARTESIAN_POINT('Ctrl Pts',(-1.97406280235204,-1.,-0.162079693556302));
#24135=CARTESIAN_POINT('Ctrl Pts',(-1.96816512678,-1.,-0.16347818545776));
#24136=CARTESIAN_POINT('Ctrl Pts',(-1.96229379940174,-1.,-0.1648165689203));
#24137=CARTESIAN_POINT('Ctrl Pts',(-1.95646759718755,-1.,-0.166093592002833));
#24138=CARTESIAN_POINT('Ctrl Pts',(-1.95069027794286,-1.,-0.167307501784469));
#24139=CARTESIAN_POINT('Ctrl Pts',(-1.94493757756879,-1.,-0.168455741607516));
#24140=CARTESIAN_POINT('Ctrl Pts',(-1.93915639211497,-1.,-0.169534904817425));
#24141=CARTESIAN_POINT('Ctrl Pts',(-1.93329183155455,-1.,-0.170541253116136));
#24142=CARTESIAN_POINT('Ctrl Pts',(-1.92731093582,-1.,-0.17147119153296));
#24143=CARTESIAN_POINT('Ctrl Pts',(-1.92122334398034,-1.,-0.172321621259557));
#24144=CARTESIAN_POINT('Ctrl Pts',(-1.91511429159681,-1.,-0.173090695383619));
#24145=CARTESIAN_POINT('Ctrl Pts',(-1.90911693975475,-1.,-0.173776635257984));
#24146=CARTESIAN_POINT('Ctrl Pts',(-1.90335253863003,-1.,-0.174375518661222));
#24147=CARTESIAN_POINT('Ctrl Pts',(-1.89788101117148,-1.,-0.174879405091277));
#24148=CARTESIAN_POINT('Ctrl Pts',(-1.89264630198279,-1.,-0.175274276190664));
#24149=CARTESIAN_POINT('Ctrl Pts',(-1.88742606272818,-1.,-0.175538155840286));
#24150=CARTESIAN_POINT('Ctrl Pts',(-1.88188663144846,-1.,-0.175644148889271));
#24151=CARTESIAN_POINT('Ctrl Pts',(-1.87563767773249,-1.,-0.175563480746205));
#24152=CARTESIAN_POINT('Ctrl Pts',(-1.86828349694972,-1.,-0.175268337590901));
#24153=CARTESIAN_POINT('Ctrl Pts',(-1.85948367089838,-1.,-0.174735259276856));
#24154=CARTESIAN_POINT('Ctrl Pts',(-1.84898113200543,-1.,-0.173946627589401));
#24155=CARTESIAN_POINT('Ctrl Pts',(-1.83658380530747,-1.,-0.17288944289442));
#24156=CARTESIAN_POINT('Ctrl Pts',(-1.82215766815414,-1.,-0.171554770207306));
#24157=CARTESIAN_POINT('Ctrl Pts',(-1.80561530633924,-1.,-0.169936923908078));
#24158=CARTESIAN_POINT('Ctrl Pts',(-1.78690649988931,-1.,-0.16803277280837));
#24159=CARTESIAN_POINT('Ctrl Pts',(-1.77018771687692,-1.,-0.166279355148738));
#24160=CARTESIAN_POINT('Ctrl Pts',(-1.75666056640041,-1.,-0.164834765708484));
#24161=CARTESIAN_POINT('Ctrl Pts',(-1.74720349503904,-1.,-0.163814161002474));
#24162=CARTESIAN_POINT('Ctrl Pts',(-1.74236521665491,-1.,-0.163289472382896));
#24163=CARTESIAN_POINT('',(-1.7075470150345,-1.,-0.383122945602004));
#24164=CARTESIAN_POINT('Origin',(0.,-1.,0.));
#24165=CARTESIAN_POINT('',(-2.11275013067528,-1.,-0.61342227326009));
#24166=CARTESIAN_POINT('Ctrl Pts',(-1.7075470150345,-1.,-0.383122945602004));
#24167=CARTESIAN_POINT('Ctrl Pts',(-1.71231062891398,-1.,-0.384119047314215));
#24168=CARTESIAN_POINT('Ctrl Pts',(-1.72162022244582,-1.,-0.386070790323281));
#24169=CARTESIAN_POINT('Ctrl Pts',(-1.73493170972829,-1.,-0.388877023502615));
#24170=CARTESIAN_POINT('Ctrl Pts',(-1.75137405310193,-1.,-0.392375812285395));
#24171=CARTESIAN_POINT('Ctrl Pts',(-1.76975560043442,-1.,-0.396346196110688));
#24172=CARTESIAN_POINT('Ctrl Pts',(-1.78598826343754,-1.,-0.399919403774155));
#24173=CARTESIAN_POINT('Ctrl Pts',(-1.80012077173238,-1.,-0.403107976163396));
#24174=CARTESIAN_POINT('Ctrl Pts',(-1.81223801812013,-1.,-0.405933518407175));
#24175=CARTESIAN_POINT('Ctrl Pts',(-1.82247022677562,-1.,-0.408428948106227));
#24176=CARTESIAN_POINT('Ctrl Pts',(-1.83100408895047,-1.,-0.410641256301276));
#24177=CARTESIAN_POINT('Ctrl Pts',(-1.8380895347617,-1.,-0.412633125322945));
#24178=CARTESIAN_POINT('Ctrl Pts',(-1.84405757074218,-1.,-0.414487438255542));
#24179=CARTESIAN_POINT('Ctrl Pts',(-1.84929312930314,-1.,-0.416300022039885));
#24180=CARTESIAN_POINT('Ctrl Pts',(-1.8541763285645,-1.,-0.418164129144045));
#24181=CARTESIAN_POINT('Ctrl Pts',(-1.8590328109667,-1.,-0.420157287975583));
#24182=CARTESIAN_POINT('Ctrl Pts',(-1.86408083333863,-1.,-0.422327307417884));
#24183=CARTESIAN_POINT('Ctrl Pts',(-1.8693780394412,-1.,-0.424678177290876));
#24184=CARTESIAN_POINT('Ctrl Pts',(-1.87486989291333,-1.,-0.427183828518743));
#24185=CARTESIAN_POINT('Ctrl Pts',(-1.88044229001778,-1.,-0.429803062482217));
#24186=CARTESIAN_POINT('Ctrl Pts',(-1.88596913666828,-1.,-0.432493038548833));
#24187=CARTESIAN_POINT('Ctrl Pts',(-1.89136993975585,-1.,-0.43522566096358));
#24188=CARTESIAN_POINT('Ctrl Pts',(-1.89663648956549,-1.,-0.437995003948443));
#24189=CARTESIAN_POINT('Ctrl Pts',(-1.90180124389137,-1.,-0.44080783370416));
#24190=CARTESIAN_POINT('Ctrl Pts',(-1.90691756144906,-1.,-0.44367755684917));
#24191=CARTESIAN_POINT('Ctrl Pts',(-1.91203699981095,-1.,-0.446617343485651));
#24192=CARTESIAN_POINT('Ctrl Pts',(-1.91718342555717,-1.,-0.449632260106572));
#24193=CARTESIAN_POINT('Ctrl Pts',(-1.9223538064847,-1.,-0.452719478359356));
#24194=CARTESIAN_POINT('Ctrl Pts',(-1.92753067150461,-1.,-0.455872005174335));
#24195=CARTESIAN_POINT('Ctrl Pts',(-1.93269066517936,-1.,-0.459081234547931));
#24196=CARTESIAN_POINT('Ctrl Pts',(-1.93781486640834,-1.,-0.462340031009087));
#24197=CARTESIAN_POINT('Ctrl Pts',(-1.94289794196205,-1.,-0.465645462026064));
#24198=CARTESIAN_POINT('Ctrl Pts',(-1.94794381136524,-1.,-0.468997482913158));
#24199=CARTESIAN_POINT('Ctrl Pts',(-1.95296148278136,-1.,-0.472397672264079));
#24200=CARTESIAN_POINT('Ctrl Pts',(-1.95796111148175,-1.,-0.475848034683171));
#24201=CARTESIAN_POINT('Ctrl Pts',(-1.96294933055938,-1.,-0.479349583074846));
#24202=CARTESIAN_POINT('Ctrl Pts',(-1.96792703422358,-1.,-0.482901662120686));
#24203=CARTESIAN_POINT('Ctrl Pts',(-1.97289186263272,-1.,-0.486502692907661));
#24204=CARTESIAN_POINT('Ctrl Pts',(-1.97783973019229,-1.,-0.490150627860955));
#24205=CARTESIAN_POINT('Ctrl Pts',(-1.9827665876182,-1.,-0.493843476541492));
#24206=CARTESIAN_POINT('Ctrl Pts',(-1.98767044752929,-1.,-0.497579909545564));
#24207=CARTESIAN_POINT('Ctrl Pts',(-1.9925514912615,-1.,-0.501359287727129));
#24208=CARTESIAN_POINT('Ctrl Pts',(-1.99741107463567,-1.,-0.505181361323011));
#24209=CARTESIAN_POINT('Ctrl Pts',(-2.00225107134733,-1.,-0.509046069886152));
#24210=CARTESIAN_POINT('Ctrl Pts',(-2.00707309946955,-1.,-0.512953306961813));
#24211=CARTESIAN_POINT('Ctrl Pts',(-2.01187773939257,-1.,-0.516902681728733));
#24212=CARTESIAN_POINT('Ctrl Pts',(-2.01666477917305,-1.,-0.520893590399428));
#24213=CARTESIAN_POINT('Ctrl Pts',(-2.02143356304712,-1.,-0.524925318333518));
#24214=CARTESIAN_POINT('Ctrl Pts',(-2.02618329083289,-1.,-0.52899712724191));
#24215=CARTESIAN_POINT('Ctrl Pts',(-2.03091336214401,-1.,-0.533108355132905));
#24216=CARTESIAN_POINT('Ctrl Pts',(-2.03562362953993,-1.,-0.537258489833134));
#24217=CARTESIAN_POINT('Ctrl Pts',(-2.0403142269048,-1.,-0.54144712061552));
#24218=CARTESIAN_POINT('Ctrl Pts',(-2.0449854471456,-1.,-0.545673903817348));
#24219=CARTESIAN_POINT('Ctrl Pts',(-2.04963761077974,-1.,-0.549938525150342));
#24220=CARTESIAN_POINT('Ctrl Pts',(-2.05427091604482,-1.,-0.554240657464109));
#24221=CARTESIAN_POINT('Ctrl Pts',(-2.05888537756571,-1.,-0.558579940185467));
#24222=CARTESIAN_POINT('Ctrl Pts',(-2.06348090160697,-1.,-0.562955993082574));
#24223=CARTESIAN_POINT('Ctrl Pts',(-2.06805732997383,-1.,-0.567368421181229));
#24224=CARTESIAN_POINT('Ctrl Pts',(-2.07261449292757,-1.,-0.571816823242411));
#24225=CARTESIAN_POINT('Ctrl Pts',(-2.07715226767361,-1.,-0.576300797416274));
#24226=CARTESIAN_POINT('Ctrl Pts',(-2.08167059018138,-1.,-0.580819952107257));
#24227=CARTESIAN_POINT('Ctrl Pts',(-2.086169437277,-1.,-0.585373918990895));
#24228=CARTESIAN_POINT('Ctrl Pts',(-2.09064881812053,-1.,-0.589962365403189));
#24229=CARTESIAN_POINT('Ctrl Pts',(-2.09510876220501,-1.,-0.594585006052823));
#24230=CARTESIAN_POINT('Ctrl Pts',(-2.09954930865331,-1.,-0.599241616422144));
#24231=CARTESIAN_POINT('Ctrl Pts',(-2.10397049887709,-1.,-0.603932030738212));
#24232=CARTESIAN_POINT('Ctrl Pts',(-2.10749199615859,-1.,-0.607711315456826));
#24233=CARTESIAN_POINT('Ctrl Pts',(-2.11012443807661,-1.,-0.610560911691113));
#24234=CARTESIAN_POINT('Ctrl Pts',(-2.11187554260142,-1.,-0.61246736556225));
#24235=CARTESIAN_POINT('Ctrl Pts',(-2.11275013067528,-1.,-0.61342227326009));
#24236=CARTESIAN_POINT('',(-2.0698113262342,-1.,-0.745574324794401));
#24237=CARTESIAN_POINT('',(-2.11275013067528,-1.,-0.61342227326009));
#24238=CARTESIAN_POINT('',(-1.60662857109684,-1.,-0.693717979106306));
#24239=CARTESIAN_POINT('Ctrl Pts',(-2.0698113262342,-1.,-0.745574324794401));
#24240=CARTESIAN_POINT('Ctrl Pts',(-2.06854248895575,-1.,-0.74583279137781));
#24241=CARTESIAN_POINT('Ctrl Pts',(-2.06600523016401,-1.,-0.746345871542695));
#24242=CARTESIAN_POINT('Ctrl Pts',(-2.06220058927162,-1.,-0.747103932785504));
#24243=CARTESIAN_POINT('Ctrl Pts',(-2.05713023030263,-1.,-0.748091554181101));
#24244=CARTESIAN_POINT('Ctrl Pts',(-2.05079645591606,-1.,-0.749287468663053));
#24245=CARTESIAN_POINT('Ctrl Pts',(-2.04446689147754,-1.,-0.750444657874758));
#24246=CARTESIAN_POINT('Ctrl Pts',(-2.03814160092173,-1.,-0.751562963361383));
#24247=CARTESIAN_POINT('Ctrl Pts',(-2.03182068456467,-1.,-0.752642180488104));
#24248=CARTESIAN_POINT('Ctrl Pts',(-2.02550428623587,-1.,-0.753682061113765));
#24249=CARTESIAN_POINT('Ctrl Pts',(-2.01919259406003,-1.,-0.75468233072352));
#24250=CARTESIAN_POINT('Ctrl Pts',(-2.01288584328149,-1.,-0.7556427049581));
#24251=CARTESIAN_POINT('Ctrl Pts',(-2.00658431587682,-1.,-0.756562904646496));
#24252=CARTESIAN_POINT('Ctrl Pts',(-2.00028834739072,-1.,-0.757442676862341));
#24253=CARTESIAN_POINT('Ctrl Pts',(-1.9939983109871,-1.,-0.758281796766377));
#24254=CARTESIAN_POINT('Ctrl Pts',(-1.98771456680806,-1.,-0.759080037802242));
#24255=CARTESIAN_POINT('Ctrl Pts',(-1.98143741418156,-1.,-0.759837147452135));
#24256=CARTESIAN_POINT('Ctrl Pts',(-1.97516705321521,-1.,-0.760552825409855));
#24257=CARTESIAN_POINT('Ctrl Pts',(-1.96890351582545,-1.,-0.761226690483986));
#24258=CARTESIAN_POINT('Ctrl Pts',(-1.96264672744229,-1.,-0.761858300014575));
#24259=CARTESIAN_POINT('Ctrl Pts',(-1.95639665309893,-1.,-0.762447203806263));
#24260=CARTESIAN_POINT('Ctrl Pts',(-1.95015342590025,-1.,-0.762992990878774));
#24261=CARTESIAN_POINT('Ctrl Pts',(-1.94391746617626,-1.,-0.76349533353858));
#24262=CARTESIAN_POINT('Ctrl Pts',(-1.93768964875867,-1.,-0.763954049121393));
#24263=CARTESIAN_POINT('Ctrl Pts',(-1.93147105496367,-1.,-0.764369010673889));
#24264=CARTESIAN_POINT('Ctrl Pts',(-1.92526263537041,-1.,-0.764740025488189));
#24265=CARTESIAN_POINT('Ctrl Pts',(-1.91906491634197,-1.,-0.765066729667095));
#24266=CARTESIAN_POINT('Ctrl Pts',(-1.91287765805174,-1.,-0.765348465884739));
#24267=CARTESIAN_POINT('Ctrl Pts',(-1.90669961402362,-1.,-0.765584196937936));
#24268=CARTESIAN_POINT('Ctrl Pts',(-1.90052930393599,-1.,-0.765772772593395));
#24269=CARTESIAN_POINT('Ctrl Pts',(-1.89436577771389,-1.,-0.765913193856979));
#24270=CARTESIAN_POINT('Ctrl Pts',(-1.88820926433409,-1.,-0.76600483706209));
#24271=CARTESIAN_POINT('Ctrl Pts',(-1.88206215302561,-1.,-0.766047794851868));
#24272=CARTESIAN_POINT('Ctrl Pts',(-1.87592888967886,-1.,-0.766042837036759));
#24273=CARTESIAN_POINT('Ctrl Pts',(-1.86981398314345,-1.,-0.765990708546111));
#24274=CARTESIAN_POINT('Ctrl Pts',(-1.86372027063314,-1.,-0.765891519092557));
#24275=CARTESIAN_POINT('Ctrl Pts',(-1.85764741390391,-1.,-0.765744212909305));
#24276=CARTESIAN_POINT('Ctrl Pts',(-1.85158945130054,-1.,-0.765545710619023));
#24277=CARTESIAN_POINT('Ctrl Pts',(-1.8455369887591,-1.,-0.765291664861971));
#24278=CARTESIAN_POINT('Ctrl Pts',(-1.83948181064823,-1.,-0.764978057881687));
#24279=CARTESIAN_POINT('Ctrl Pts',(-1.8334207722714,-1.,-0.764602549687845));
#24280=CARTESIAN_POINT('Ctrl Pts',(-1.8273599120008,-1.,-0.764165902606055));
#24281=CARTESIAN_POINT('Ctrl Pts',(-1.82131873145297,-1.,-0.763673465462854));
#24282=CARTESIAN_POINT('Ctrl Pts',(-1.81532118405566,-1.,-0.763132003836783));
#24283=CARTESIAN_POINT('Ctrl Pts',(-1.80938551463989,-1.,-0.762546129464036));
#24284=CARTESIAN_POINT('Ctrl Pts',(-1.80351583877334,-1.,-0.761915336443515));
#24285=CARTESIAN_POINT('Ctrl Pts',(-1.79768986997735,-1.,-0.761229695230359));
#24286=CARTESIAN_POINT('Ctrl Pts',(-1.79185815610802,-1.,-0.760469555880425));
#24287=CARTESIAN_POINT('Ctrl Pts',(-1.78596964884526,-1.,-0.759614401109868));
#24288=CARTESIAN_POINT('Ctrl Pts',(-1.77999411220912,-1.,-0.75865062667738));
#24289=CARTESIAN_POINT('Ctrl Pts',(-1.77394167108342,-1.,-0.757578264077238));
#24290=CARTESIAN_POINT('Ctrl Pts',(-1.76789396003141,-1.,-0.756421896028403));
#24291=CARTESIAN_POINT('Ctrl Pts',(-1.7619781724032,-1.,-0.755220979975262));
#24292=CARTESIAN_POINT('Ctrl Pts',(-1.75631083600175,-1.,-0.75400925402848));
#24293=CARTESIAN_POINT('Ctrl Pts',(-1.75095139468809,-1.,-0.752797683531377));
#24294=CARTESIAN_POINT('Ctrl Pts',(-1.74585086852298,-1.,-0.751555614163629));
#24295=CARTESIAN_POINT('Ctrl Pts',(-1.74080458266705,-1.,-0.75019343597954));
#24296=CARTESIAN_POINT('Ctrl Pts',(-1.73550351679848,-1.,-0.748582462954854));
#24297=CARTESIAN_POINT('Ctrl Pts',(-1.72958533647399,-1.,-0.746574710096436));
#24298=CARTESIAN_POINT('Ctrl Pts',(-1.7226822991693,-1.,-0.744021445433764));
#24299=CARTESIAN_POINT('Ctrl Pts',(-1.71447789751927,-1.,-0.740795162032087));
#24300=CARTESIAN_POINT('Ctrl Pts',(-1.70473309006121,-1.,-0.736799665724771));
#24301=CARTESIAN_POINT('Ctrl Pts',(-1.69326921975743,-1.,-0.731963238697195));
#24302=CARTESIAN_POINT('Ctrl Pts',(-1.67996158455503,-1.,-0.726235967997433));
#24303=CARTESIAN_POINT('Ctrl Pts',(-1.6647288055568,-1.,-0.719585433804282));
#24304=CARTESIAN_POINT('Ctrl Pts',(-1.64752408832016,-1.,-0.711993139355394));
#24305=CARTESIAN_POINT('Ctrl Pts',(-1.63216541664676,-1.,-0.705159151988319));
#24306=CARTESIAN_POINT('Ctrl Pts',(-1.61974673472612,-1.,-0.699605146405088));
#24307=CARTESIAN_POINT('Ctrl Pts',(-1.61106790958151,-1.,-0.695712097881194));
#24308=CARTESIAN_POINT('Ctrl Pts',(-1.60662857109684,-1.,-0.693717979106306));
#24309=CARTESIAN_POINT('',(-1.5055822144029,-1.,-0.892032620296855));
#24310=CARTESIAN_POINT('Origin',(0.,-1.,0.));
#24311=CARTESIAN_POINT('',(-1.81978687191668,-1.,-1.23627494547115));
#24312=CARTESIAN_POINT('Ctrl Pts',(-1.5055822144029,-1.,-0.892032620296855));
#24313=CARTESIAN_POINT('Ctrl Pts',(-1.50980486806688,-1.,-0.894452006964543));
#24314=CARTESIAN_POINT('Ctrl Pts',(-1.51805569590094,-1.,-0.899185047483511));
#24315=CARTESIAN_POINT('Ctrl Pts',(-1.52984849887993,-1.,-0.905967409625651));
#24316=CARTESIAN_POINT('Ctrl Pts',(-1.54440491149498,-1.,-0.914375919026456));
#24317=CARTESIAN_POINT('Ctrl Pts',(-1.56065988578893,-1.,-0.923832188944341));
#24318=CARTESIAN_POINT('Ctrl Pts',(-1.57499388382243,-1.,-0.932246680108685));
#24319=CARTESIAN_POINT('Ctrl Pts',(-1.58744937487176,-1.,-0.939646377893399));
#24320=CARTESIAN_POINT('Ctrl Pts',(-1.59810042043673,-1.,-0.946078063315257));
#24321=CARTESIAN_POINT('Ctrl Pts',(-1.60706069896936,-1.,-0.951613284356035));
#24322=CARTESIAN_POINT('Ctrl Pts',(-1.61449324337085,-1.,-0.956354422920671));
#24323=CARTESIAN_POINT('Ctrl Pts',(-1.62061638140221,-1.,-0.960438326101729));
#24324=CARTESIAN_POINT('Ctrl Pts',(-1.62571930670187,-1.,-0.964046107040536));
#24325=CARTESIAN_POINT('Ctrl Pts',(-1.63013849959461,-1.,-0.967387853230345));
#24326=CARTESIAN_POINT('Ctrl Pts',(-1.63420665729798,-1.,-0.970669715997509));
#24327=CARTESIAN_POINT('Ctrl Pts',(-1.63820952658144,-1.,-0.974066058287418));
#24328=CARTESIAN_POINT('Ctrl Pts',(-1.64233990826687,-1.,-0.977689794119416));
#24329=CARTESIAN_POINT('Ctrl Pts',(-1.64665139190656,-1.,-0.981562530939489));
#24330=CARTESIAN_POINT('Ctrl Pts',(-1.65110016612638,-1.,-0.985642622920821));
#24331=CARTESIAN_POINT('Ctrl Pts',(-1.65559044289699,-1.,-0.989855627854165));
#24332=CARTESIAN_POINT('Ctrl Pts',(-1.66001553809947,-1.,-0.994121836661306));
#24333=CARTESIAN_POINT('Ctrl Pts',(-1.66430758030376,-1.,-0.998389654952758));
#24334=CARTESIAN_POINT('Ctrl Pts',(-1.66846059277303,-1.,-1.00265091003727));
#24335=CARTESIAN_POINT('Ctrl Pts',(-1.67250335383293,-1.,-1.00692206696414));
#24336=CARTESIAN_POINT('Ctrl Pts',(-1.67648246776464,-1.,-1.01123236493511));
#24337=CARTESIAN_POINT('Ctrl Pts',(-1.68044289894798,-1.,-1.01561026162773));
#24338=CARTESIAN_POINT('Ctrl Pts',(-1.68440578021706,-1.,-1.02006795074201));
#24339=CARTESIAN_POINT('Ctrl Pts',(-1.68836910178447,-1.,-1.02460180535255));
#24340=CARTESIAN_POINT('Ctrl Pts',(-1.69231840863458,-1.,-1.02919977579147));
#24341=CARTESIAN_POINT('Ctrl Pts',(-1.69623414782771,-1.,-1.03384646003588));
#24342=CARTESIAN_POINT('Ctrl Pts',(-1.70010052930962,-1.,-1.03852922490789));
#24343=CARTESIAN_POINT('Ctrl Pts',(-1.70391338707982,-1.,-1.04324363334554));
#24344=CARTESIAN_POINT('Ctrl Pts',(-1.70767646263649,-1.,-1.04799085404995));
#24345=CARTESIAN_POINT('Ctrl Pts',(-1.71139783543989,-1.,-1.05277517202855));
#24346=CARTESIAN_POINT('Ctrl Pts',(-1.7150865442702,-1.,-1.05760163192479));
#24347=CARTESIAN_POINT('Ctrl Pts',(-1.71874858456904,-1.,-1.06247324680647));
#24348=CARTESIAN_POINT('Ctrl Pts',(-1.72238500928453,-1.,-1.06738966975462));
#24349=CARTESIAN_POINT('Ctrl Pts',(-1.72599406198488,-1.,-1.07234866990252));
#24350=CARTESIAN_POINT('Ctrl Pts',(-1.72957248977424,-1.,-1.0773470373727));
#24351=CARTESIAN_POINT('Ctrl Pts',(-1.73311705663407,-1.,-1.08238162784749));
#24352=CARTESIAN_POINT('Ctrl Pts',(-1.73662628326091,-1.,-1.08745056285427));
#24353=CARTESIAN_POINT('Ctrl Pts',(-1.74010053962247,-1.,-1.09255329056493));
#24354=CARTESIAN_POINT('Ctrl Pts',(-1.74354119236208,-1.,-1.09768999241225));
#24355=CARTESIAN_POINT('Ctrl Pts',(-1.74695004214923,-1.,-1.10286118991143));
#24356=CARTESIAN_POINT('Ctrl Pts',(-1.7503286607592,-1.,-1.10806728183007));
#24357=CARTESIAN_POINT('Ctrl Pts',(-1.7536777209463,-1.,-1.11330807582551));
#24358=CARTESIAN_POINT('Ctrl Pts',(-1.75699720772105,-1.,-1.11858293216763));
#24359=CARTESIAN_POINT('Ctrl Pts',(-1.76028671825096,-1.,-1.12389096855086));
#24360=CARTESIAN_POINT('Ctrl Pts',(-1.7635457196617,-1.,-1.12923123555075));
#24361=CARTESIAN_POINT('Ctrl Pts',(-1.76677384551862,-1.,-1.1346029180462));
#24362=CARTESIAN_POINT('Ctrl Pts',(-1.76997111386769,-1.,-1.14000548336975));
#24363=CARTESIAN_POINT('Ctrl Pts',(-1.77313777896194,-1.,-1.1454385822692));
#24364=CARTESIAN_POINT('Ctrl Pts',(-1.7762742255701,-1.,-1.15090197841515));
#24365=CARTESIAN_POINT('Ctrl Pts',(-1.77938085564275,-1.,-1.15639547194698));
#24366=CARTESIAN_POINT('Ctrl Pts',(-1.78245795881009,-1.,-1.16191881298499));
#24367=CARTESIAN_POINT('Ctrl Pts',(-1.78550566040443,-1.,-1.16747166312303));
#24368=CARTESIAN_POINT('Ctrl Pts',(-1.78852398877616,-1.,-1.17305363177328));
#24369=CARTESIAN_POINT('Ctrl Pts',(-1.79151291552689,-1.,-1.17866429440809));
#24370=CARTESIAN_POINT('Ctrl Pts',(-1.79447240321515,-1.,-1.18430321697432));
#24371=CARTESIAN_POINT('Ctrl Pts',(-1.79740245923478,-1.,-1.18996997934445));
#24372=CARTESIAN_POINT('Ctrl Pts',(-1.80030314369879,-1.,-1.19566418930242));
#24373=CARTESIAN_POINT('Ctrl Pts',(-1.80317454838603,-1.,-1.20138548938974));
#24374=CARTESIAN_POINT('Ctrl Pts',(-1.80601678480707,-1.,-1.20713356605475));
#24375=CARTESIAN_POINT('Ctrl Pts',(-1.80882996917129,-1.,-1.21290815708314));
#24376=CARTESIAN_POINT('Ctrl Pts',(-1.81161420806656,-1.,-1.21870906103557));
#24377=CARTESIAN_POINT('Ctrl Pts',(-1.81436959210434,-1.,-1.2245361330495));
#24378=CARTESIAN_POINT('Ctrl Pts',(-1.8165508718364,-1.,-1.2292186489137));
#24379=CARTESIAN_POINT('Ctrl Pts',(-1.81817389921279,-1.,-1.2327422452705));
#24380=CARTESIAN_POINT('Ctrl Pts',(-1.81925017193666,-1.,-1.23509651170476));
#24381=CARTESIAN_POINT('Ctrl Pts',(-1.81978687191668,-1.,-1.23627494547115));
#24382=CARTESIAN_POINT('',(-1.73811241238545,-1.,-1.34869019493419));
#24383=CARTESIAN_POINT('',(-1.81978687191668,-1.,-1.23627494547115));
#24384=CARTESIAN_POINT('',(-1.31362392696032,-1.,-1.15624053661742));
#24385=CARTESIAN_POINT('Ctrl Pts',(-1.73811241238545,-1.,-1.34869019493419));
#24386=CARTESIAN_POINT('Ctrl Pts',(-1.73682580585691,-1.,-1.34854391898045));
#24387=CARTESIAN_POINT('Ctrl Pts',(-1.73425417885907,-1.,-1.34824783112887));
#24388=CARTESIAN_POINT('Ctrl Pts',(-1.7304014965394,-1.,-1.34779309152035));
#24389=CARTESIAN_POINT('Ctrl Pts',(-1.72527410680674,-1.,-1.34716554819527));
#24390=CARTESIAN_POINT('Ctrl Pts',(-1.7188807715049,-1.,-1.34634568653227));
#24391=CARTESIAN_POINT('Ctrl Pts',(-1.71250340686822,-1.,-1.34549029589416));
#24392=CARTESIAN_POINT('Ctrl Pts',(-1.70614212266738,-1.,-1.34459924533831));
#24393=CARTESIAN_POINT('Ctrl Pts',(-1.69979707754427,-1.,-1.34367237124483));
#24394=CARTESIAN_POINT('Ctrl Pts',(-1.6934684849687,-1.,-1.34270948206319));
#24395=CARTESIAN_POINT('Ctrl Pts',(-1.68715660868764,-1.,-1.341710374848));
#24396=CARTESIAN_POINT('Ctrl Pts',(-1.68086176030362,-1.,-1.34067485185203));
#24397=CARTESIAN_POINT('Ctrl Pts',(-1.67458429426086,-1.,-1.3396027347034));
#24398=CARTESIAN_POINT('Ctrl Pts',(-1.66832460783989,-1.,-1.33849388654388));
#24399=CARTESIAN_POINT('Ctrl Pts',(-1.66208312541983,-1.,-1.33734820885262));
#24400=CARTESIAN_POINT('Ctrl Pts',(-1.65586025952593,-1.,-1.33616559745172));
#24401=CARTESIAN_POINT('Ctrl Pts',(-1.6496563728683,-1.,-1.33494590467993));
#24402=CARTESIAN_POINT('Ctrl Pts',(-1.6434717485603,-1.,-1.33368890676572));
#24403=CARTESIAN_POINT('Ctrl Pts',(-1.63730653475089,-1.,-1.33239425103724));
#24404=CARTESIAN_POINT('Ctrl Pts',(-1.63116079730923,-1.,-1.33106149345645));
#24405=CARTESIAN_POINT('Ctrl Pts',(-1.62503464209797,-1.,-1.3296901950568));
#24406=CARTESIAN_POINT('Ctrl Pts',(-1.61892832270724,-1.,-1.32828000610449));
#24407=CARTESIAN_POINT('Ctrl Pts',(-1.6128423401575,-1.,-1.32683074483356));
#24408=CARTESIAN_POINT('Ctrl Pts',(-1.60677758290954,-1.,-1.32534250785782));
#24409=CARTESIAN_POINT('Ctrl Pts',(-1.60073511858687,-1.,-1.32381550858256));
#24410=CARTESIAN_POINT('Ctrl Pts',(-1.59471591079403,-1.,-1.32224985747682));
#24411=CARTESIAN_POINT('Ctrl Pts',(-1.58872057258245,-1.,-1.32064537110892));
#24412=CARTESIAN_POINT('Ctrl Pts',(-1.58274907898834,-1.,-1.31900135021432));
#24413=CARTESIAN_POINT('Ctrl Pts',(-1.5768005650559,-1.,-1.31731642317187));
#24414=CARTESIAN_POINT('Ctrl Pts',(-1.57087397835723,-1.,-1.31558903860016));
#24415=CARTESIAN_POINT('Ctrl Pts',(-1.56496872402353,-1.,-1.31381795281002));
#24416=CARTESIAN_POINT('Ctrl Pts',(-1.55908521254821,-1.,-1.31200264341696));
#24417=CARTESIAN_POINT('Ctrl Pts',(-1.55322568759481,-1.,-1.31014393684222));
#24418=CARTESIAN_POINT('Ctrl Pts',(-1.54739413957185,-1.,-1.30824393907473));
#24419=CARTESIAN_POINT('Ctrl Pts',(-1.54159462645432,-1.,-1.30630475189556));
#24420=CARTESIAN_POINT('Ctrl Pts',(-1.53582981268977,-1.,-1.30432735639489));
#24421=CARTESIAN_POINT('Ctrl Pts',(-1.53009970283891,-1.,-1.30231064395568));
#24422=CARTESIAN_POINT('Ctrl Pts',(-1.52439957861062,-1.,-1.30024984366328));
#24423=CARTESIAN_POINT('Ctrl Pts',(-1.51872184912724,-1.,-1.29813791800747));
#24424=CARTESIAN_POINT('Ctrl Pts',(-1.51305994241402,-1.,-1.29596850710509));
#24425=CARTESIAN_POINT('Ctrl Pts',(-1.50741159078365,-1.,-1.29373841372842));
#24426=CARTESIAN_POINT('Ctrl Pts',(-1.50178230149776,-1.,-1.29145022885181));
#24427=CARTESIAN_POINT('Ctrl Pts',(-1.49618896881754,-1.,-1.28911506584254));
#24428=CARTESIAN_POINT('Ctrl Pts',(-1.4906522831278,-1.,-1.2867467611644));
#24429=CARTESIAN_POINT('Ctrl Pts',(-1.4851881711891,-1.,-1.28435533880201));
#24430=CARTESIAN_POINT('Ctrl Pts',(-1.47980070347095,-1.,-1.28194158939517));
#24431=CARTESIAN_POINT('Ctrl Pts',(-1.4744717526707,-1.,-1.2794891824849));
#24432=CARTESIAN_POINT('Ctrl Pts',(-1.46916035917133,-1.,-1.27696414831089));
#24433=CARTESIAN_POINT('Ctrl Pts',(-1.46382431332476,-1.,-1.27433119897822));
#24434=CARTESIAN_POINT('Ctrl Pts',(-1.45843906294697,-1.,-1.27156805265289));
#24435=CARTESIAN_POINT('Ctrl Pts',(-1.45301422764247,-1.,-1.2686778680489));
#24436=CARTESIAN_POINT('Ctrl Pts',(-1.44761985001662,-1.,-1.26570925118868));
#24437=CARTESIAN_POINT('Ctrl Pts',(-1.44236470511303,-1.,-1.26273903323859));
#24438=CARTESIAN_POINT('Ctrl Pts',(-1.43734919180848,-1.,-1.25983531012005));
#24439=CARTESIAN_POINT('Ctrl Pts',(-1.43262645609691,-1.,-1.25702687965755));
#24440=CARTESIAN_POINT('Ctrl Pts',(-1.42815938799387,-1.,-1.25426945222639));
#24441=CARTESIAN_POINT('Ctrl Pts',(-1.42378102115575,-1.,-1.2514145557001));
#24442=CARTESIAN_POINT('Ctrl Pts',(-1.41923722596025,-1.,-1.24824430986571));
#24443=CARTESIAN_POINT('Ctrl Pts',(-1.41422913175179,-1.,-1.24450600513056));
#24444=CARTESIAN_POINT('Ctrl Pts',(-1.40845295531283,-1.,-1.23994455029534));
#24445=CARTESIAN_POINT('Ctrl Pts',(-1.40164708206106,-1.,-1.23434087290423));
#24446=CARTESIAN_POINT('Ctrl Pts',(-1.39361389568796,-1.,-1.22752961899387));
#24447=CARTESIAN_POINT('Ctrl Pts',(-1.38420564527715,-1.,-1.21938737280852));
#24448=CARTESIAN_POINT('Ctrl Pts',(-1.37331915607905,-1.,-1.20982812925645));
#24449=CARTESIAN_POINT('Ctrl Pts',(-1.36088705043885,-1.,-1.1987959077932));
#24450=CARTESIAN_POINT('Ctrl Pts',(-1.34687054001093,-1.,-1.18625865667441));
#24451=CARTESIAN_POINT('Ctrl Pts',(-1.33437539347008,-1.,-1.17501305789857));
#24452=CARTESIAN_POINT('Ctrl Pts',(-1.32428080721772,-1.,-1.16589330093588));
#24453=CARTESIAN_POINT('Ctrl Pts',(-1.31722977216397,-1.,-1.15950888730809));
#24454=CARTESIAN_POINT('Ctrl Pts',(-1.31362392696032,-1.,-1.15624053661742));
#24455=CARTESIAN_POINT('',(-1.15624053661742,-1.,-1.31362392696033));
#24456=CARTESIAN_POINT('Origin',(0.,-1.,0.));
#24457=CARTESIAN_POINT('',(-1.34869019493419,-1.,-1.73811241238545));
#24458=CARTESIAN_POINT('Ctrl Pts',(-1.15624053661742,-1.,-1.31362392696033));
#24459=CARTESIAN_POINT('Ctrl Pts',(-1.15950888730433,-1.,-1.3172297721596));
#24460=CARTESIAN_POINT('Ctrl Pts',(-1.16589330092532,-1.,-1.32428080720544));
#24461=CARTESIAN_POINT('Ctrl Pts',(-1.17501305787994,-1.,-1.33437539344842));
#24462=CARTESIAN_POINT('Ctrl Pts',(-1.18625865664915,-1.,-1.34687053998157));
#24463=CARTESIAN_POINT('Ctrl Pts',(-1.1987959077656,-1.,-1.36088705040677));
#24464=CARTESIAN_POINT('Ctrl Pts',(-1.20982812923113,-1.,-1.37331915604962));
#24465=CARTESIAN_POINT('Ctrl Pts',(-1.21938737278853,-1.,-1.38420564525391));
#24466=CARTESIAN_POINT('Ctrl Pts',(-1.22752961898063,-1.,-1.39361389567257));
#24467=CARTESIAN_POINT('Ctrl Pts',(-1.23434087289768,-1.,-1.40164708205345));
#24468=CARTESIAN_POINT('Ctrl Pts',(-1.23994455029421,-1.,-1.40845295531151));
#24469=CARTESIAN_POINT('Ctrl Pts',(-1.24450600513278,-1.,-1.41422913175437));
#24470=CARTESIAN_POINT('Ctrl Pts',(-1.24824430986911,-1.,-1.41923722596421));
#24471=CARTESIAN_POINT('Ctrl Pts',(-1.25141455570299,-1.,-1.42378102115911));
#24472=CARTESIAN_POINT('Ctrl Pts',(-1.25426945222783,-1.,-1.42815938799555));
#24473=CARTESIAN_POINT('Ctrl Pts',(-1.25702687965744,-1.,-1.43262645609679));
#24474=CARTESIAN_POINT('Ctrl Pts',(-1.25983531011894,-1.,-1.43734919180719));
#24475=CARTESIAN_POINT('Ctrl Pts',(-1.26273903323723,-1.,-1.44236470511145));
#24476=CARTESIAN_POINT('Ctrl Pts',(-1.26570925118767,-1.,-1.44761985001544));
#24477=CARTESIAN_POINT('Ctrl Pts',(-1.26867786804854,-1.,-1.45301422764205));
#24478=CARTESIAN_POINT('Ctrl Pts',(-1.27156805265312,-1.,-1.45843906294725));
#24479=CARTESIAN_POINT('Ctrl Pts',(-1.27433119897877,-1.,-1.4638243133254));
#24480=CARTESIAN_POINT('Ctrl Pts',(-1.27696414831144,-1.,-1.46916035917197));
#24481=CARTESIAN_POINT('Ctrl Pts',(-1.27948918248524,-1.,-1.4744717526711));
#24482=CARTESIAN_POINT('Ctrl Pts',(-1.28194158939522,-1.,-1.47980070347102));
#24483=CARTESIAN_POINT('Ctrl Pts',(-1.28435533880184,-1.,-1.48518817118891));
#24484=CARTESIAN_POINT('Ctrl Pts',(-1.28674676116415,-1.,-1.4906522831275));
#24485=CARTESIAN_POINT('Ctrl Pts',(-1.28911506584232,-1.,-1.49618896881729));
#24486=CARTESIAN_POINT('Ctrl Pts',(-1.29145022885171,-1.,-1.50178230149764));
#24487=CARTESIAN_POINT('Ctrl Pts',(-1.29373841372843,-1.,-1.50741159078367));
#24488=CARTESIAN_POINT('Ctrl Pts',(-1.29596850710518,-1.,-1.51305994241412));
#24489=CARTESIAN_POINT('Ctrl Pts',(-1.29813791800757,-1.,-1.51872184912735));
#24490=CARTESIAN_POINT('Ctrl Pts',(-1.30024984366334,-1.,-1.5243995786107));
#24491=CARTESIAN_POINT('Ctrl Pts',(-1.3023106439557,-1.,-1.53009970283893));
#24492=CARTESIAN_POINT('Ctrl Pts',(-1.30432735639487,-1.,-1.53582981268976));
#24493=CARTESIAN_POINT('Ctrl Pts',(-1.30630475189553,-1.,-1.54159462645428));
#24494=CARTESIAN_POINT('Ctrl Pts',(-1.30824393907471,-1.,-1.54739413957183));
#24495=CARTESIAN_POINT('Ctrl Pts',(-1.31014393684221,-1.,-1.55322568759481));
#24496=CARTESIAN_POINT('Ctrl Pts',(-1.31200264341696,-1.,-1.55908521254822));
#24497=CARTESIAN_POINT('Ctrl Pts',(-1.31381795281002,-1.,-1.56496872402352));
#24498=CARTESIAN_POINT('Ctrl Pts',(-1.31558903860015,-1.,-1.57087397835721));
#24499=CARTESIAN_POINT('Ctrl Pts',(-1.31731642317183,-1.,-1.57680056505585));
#24500=CARTESIAN_POINT('Ctrl Pts',(-1.31900135021428,-1.,-1.58274907898829));
#24501=CARTESIAN_POINT('Ctrl Pts',(-1.32064537110891,-1.,-1.58872057258244));
#24502=CARTESIAN_POINT('Ctrl Pts',(-1.32224985747686,-1.,-1.59471591079408));
#24503=CARTESIAN_POINT('Ctrl Pts',(-1.32381550858266,-1.,-1.600735118587));
#24504=CARTESIAN_POINT('Ctrl Pts',(-1.32534250785794,-1.,-1.6067775829097));
#24505=CARTESIAN_POINT('Ctrl Pts',(-1.32683074483365,-1.,-1.61284234015762));
#24506=CARTESIAN_POINT('Ctrl Pts',(-1.32828000610448,-1.,-1.61892832270723));
#24507=CARTESIAN_POINT('Ctrl Pts',(-1.32969019505665,-1.,-1.62503464209777));
#24508=CARTESIAN_POINT('Ctrl Pts',(-1.33106149345618,-1.,-1.63116079730887));
#24509=CARTESIAN_POINT('Ctrl Pts',(-1.33239425103694,-1.,-1.6373065347505));
#24510=CARTESIAN_POINT('Ctrl Pts',(-1.33368890676554,-1.,-1.64347174856007));
#24511=CARTESIAN_POINT('Ctrl Pts',(-1.33494590468003,-1.,-1.64965637286843));
#24512=CARTESIAN_POINT('Ctrl Pts',(-1.33616559745217,-1.,-1.65586025952651));
#24513=CARTESIAN_POINT('Ctrl Pts',(-1.33734820885331,-1.,-1.66208312542073));
#24514=CARTESIAN_POINT('Ctrl Pts',(-1.33849388654458,-1.,-1.66832460784078));
#24515=CARTESIAN_POINT('Ctrl Pts',(-1.33960273470372,-1.,-1.67458429426126));
#24516=CARTESIAN_POINT('Ctrl Pts',(-1.3406748518516,-1.,-1.68086176030308));
#24517=CARTESIAN_POINT('Ctrl Pts',(-1.34171037484673,-1.,-1.68715660868602));
#24518=CARTESIAN_POINT('Ctrl Pts',(-1.34270948206139,-1.,-1.6934684849664));
#24519=CARTESIAN_POINT('Ctrl Pts',(-1.34367237124322,-1.,-1.69979707754221));
#24520=CARTESIAN_POINT('Ctrl Pts',(-1.34459924533783,-1.,-1.70614212266676));
#24521=CARTESIAN_POINT('Ctrl Pts',(-1.34549029589563,-1.,-1.71250340687011));
#24522=CARTESIAN_POINT('Ctrl Pts',(-1.34634568653586,-1.,-1.7188807715095));
#24523=CARTESIAN_POINT('Ctrl Pts',(-1.34716554820013,-1.,-1.72527410681298));
#24524=CARTESIAN_POINT('Ctrl Pts',(-1.3477930915247,-1.,-1.73040149654497));
#24525=CARTESIAN_POINT('Ctrl Pts',(-1.34824783113158,-1.,-1.73425417886255));
#24526=CARTESIAN_POINT('Ctrl Pts',(-1.34854391898145,-1.,-1.73682580585819));
#24527=CARTESIAN_POINT('Ctrl Pts',(-1.34869019493419,-1.,-1.73811241238545));
#24528=CARTESIAN_POINT('',(-1.23627494547115,-1.,-1.81978687191668));
#24529=CARTESIAN_POINT('',(-1.34869019493419,-1.,-1.73811241238545));
#24530=CARTESIAN_POINT('',(-0.892032620296855,-1.,-1.5055822144029));
#24531=CARTESIAN_POINT('Ctrl Pts',(-1.23627494547115,-1.,-1.81978687191668));
#24532=CARTESIAN_POINT('Ctrl Pts',(-1.23509651170384,-1.,-1.81925017193531));
#24533=CARTESIAN_POINT('Ctrl Pts',(-1.23274224526804,-1.,-1.81817389920914));
#24534=CARTESIAN_POINT('Ctrl Pts',(-1.22921864890975,-1.,-1.81655087183054));
#24535=CARTESIAN_POINT('Ctrl Pts',(-1.22453613304507,-1.,-1.81436959209778));
#24536=CARTESIAN_POINT('Ctrl Pts',(-1.2187090610323,-1.,-1.81161420806172));
#24537=CARTESIAN_POINT('Ctrl Pts',(-1.2129081570818,-1.,-1.80882996916931));
#24538=CARTESIAN_POINT('Ctrl Pts',(-1.20713356605519,-1.,-1.80601678480772));
#24539=CARTESIAN_POINT('Ctrl Pts',(-1.2013854893912,-1.,-1.8031745483882));
#24540=CARTESIAN_POINT('Ctrl Pts',(-1.19566418930405,-1.,-1.80030314370121));
#24541=CARTESIAN_POINT('Ctrl Pts',(-1.1899699793456,-1.,-1.79740245923649));
#24542=CARTESIAN_POINT('Ctrl Pts',(-1.18430321697471,-1.,-1.79447240321572));
#24543=CARTESIAN_POINT('Ctrl Pts',(-1.17866429440781,-1.,-1.79151291552646));
#24544=CARTESIAN_POINT('Ctrl Pts',(-1.17305363177265,-1.,-1.78852398877523));
#24545=CARTESIAN_POINT('Ctrl Pts',(-1.16747166312239,-1.,-1.78550566040349));
#24546=CARTESIAN_POINT('Ctrl Pts',(-1.16191881298458,-1.,-1.78245795880949));
#24547=CARTESIAN_POINT('Ctrl Pts',(-1.15639547194689,-1.,-1.77938085564261));
#24548=CARTESIAN_POINT('Ctrl Pts',(-1.15090197841531,-1.,-1.77627422557034));
#24549=CARTESIAN_POINT('Ctrl Pts',(-1.14543858226948,-1.,-1.77313777896234));
#24550=CARTESIAN_POINT('Ctrl Pts',(-1.14000548337,-1.,-1.76997111386806));
#24551=CARTESIAN_POINT('Ctrl Pts',(-1.13460291804635,-1.,-1.76677384551883));
#24552=CARTESIAN_POINT('Ctrl Pts',(-1.12923123555076,-1.,-1.76354571966171));
#24553=CARTESIAN_POINT('Ctrl Pts',(-1.12389096855078,-1.,-1.76028671825084));
#24554=CARTESIAN_POINT('Ctrl Pts',(-1.11858293216752,-1.,-1.75699720772089));
#24555=CARTESIAN_POINT('Ctrl Pts',(-1.11330807582542,-1.,-1.75367772094617));
#24556=CARTESIAN_POINT('Ctrl Pts',(-1.10806728183003,-1.,-1.75032866075914));
#24557=CARTESIAN_POINT('Ctrl Pts',(-1.10286118991144,-1.,-1.74695004214924));
#24558=CARTESIAN_POINT('Ctrl Pts',(-1.09768999241229,-1.,-1.74354119236212));
#24559=CARTESIAN_POINT('Ctrl Pts',(-1.09255329056496,-1.,-1.74010053962252));
#24560=CARTESIAN_POINT('Ctrl Pts',(-1.08745056285429,-1.,-1.73662628326093));
#24561=CARTESIAN_POINT('Ctrl Pts',(-1.08238162784749,-1.,-1.73311705663407));
#24562=CARTESIAN_POINT('Ctrl Pts',(-1.0773470373727,-1.,-1.72957248977424));
#24563=CARTESIAN_POINT('Ctrl Pts',(-1.07234866990252,-1.,-1.72599406198489));
#24564=CARTESIAN_POINT('Ctrl Pts',(-1.06738966975463,-1.,-1.72238500928456));
#24565=CARTESIAN_POINT('Ctrl Pts',(-1.0624732468065,-1.,-1.71874858456908));
#24566=CARTESIAN_POINT('Ctrl Pts',(-1.05760163192481,-1.,-1.71508654427022));
#24567=CARTESIAN_POINT('Ctrl Pts',(-1.05277517202854,-1.,-1.71139783543986));
#24568=CARTESIAN_POINT('Ctrl Pts',(-1.0479908540499,-1.,-1.70767646263641));
#24569=CARTESIAN_POINT('Ctrl Pts',(-1.04324363334546,-1.,-1.70391338707969));
#24570=CARTESIAN_POINT('Ctrl Pts',(-1.03852922490782,-1.,-1.70010052930951));
#24571=CARTESIAN_POINT('Ctrl Pts',(-1.03384646003587,-1.,-1.69623414782769));
#24572=CARTESIAN_POINT('Ctrl Pts',(-1.02919977579155,-1.,-1.69231840863471));
#24573=CARTESIAN_POINT('Ctrl Pts',(-1.02460180535272,-1.,-1.68836910178475));
#24574=CARTESIAN_POINT('Ctrl Pts',(-1.02006795074222,-1.,-1.68440578021739));
#24575=CARTESIAN_POINT('Ctrl Pts',(-1.01561026162787,-1.,-1.6804428989482));
#24576=CARTESIAN_POINT('Ctrl Pts',(-1.01123236493507,-1.,-1.67648246776457));
#24577=CARTESIAN_POINT('Ctrl Pts',(-1.00692206696387,-1.,-1.67250335383248));
#24578=CARTESIAN_POINT('Ctrl Pts',(-1.00265091003682,-1.,-1.66846059277231));
#24579=CARTESIAN_POINT('Ctrl Pts',(-0.998389654952317,-1.,-1.66430758030304));
#24580=CARTESIAN_POINT('Ctrl Pts',(-0.994121836661116,-1.,-1.66001553809916));
#24581=CARTESIAN_POINT('Ctrl Pts',(-0.98985562785445,-1.,-1.65559044289746));
#24582=CARTESIAN_POINT('Ctrl Pts',(-0.985642622921626,-1.,-1.6511001661277));
#24583=CARTESIAN_POINT('Ctrl Pts',(-0.981562530940574,-1.,-1.64665139190834));
#24584=CARTESIAN_POINT('Ctrl Pts',(-0.977689794120297,-1.,-1.64233990826831));
#24585=CARTESIAN_POINT('Ctrl Pts',(-0.974066058287501,-1.,-1.63820952658157));
#24586=CARTESIAN_POINT('Ctrl Pts',(-0.970669715996356,-1.,-1.63420665729609));
#24587=CARTESIAN_POINT('Ctrl Pts',(-0.967387853228041,-1.,-1.63013849959083));
#24588=CARTESIAN_POINT('Ctrl Pts',(-0.964046107037821,-1.,-1.6257193066974));
#24589=CARTESIAN_POINT('Ctrl Pts',(-0.960438326099958,-1.,-1.62061638139929));
#24590=CARTESIAN_POINT('Ctrl Pts',(-0.956354422921573,-1.,-1.61449324337233));
#24591=CARTESIAN_POINT('Ctrl Pts',(-0.951613284361248,-1.,-1.60706069897794));
#24592=CARTESIAN_POINT('Ctrl Pts',(-0.946078063325796,-1.,-1.59810042045408));
#24593=CARTESIAN_POINT('Ctrl Pts',(-0.939646377909319,-1.,-1.58744937489796));
#24594=CARTESIAN_POINT('Ctrl Pts',(-0.932246680128849,-1.,-1.57499388385561));
#24595=CARTESIAN_POINT('Ctrl Pts',(-0.923832188966322,-1.,-1.56065988582509));
#24596=CARTESIAN_POINT('Ctrl Pts',(-0.91437591904658,-1.,-1.54440491152808));
#24597=CARTESIAN_POINT('Ctrl Pts',(-0.905967409640499,-1.,-1.52984849890434));
#24598=CARTESIAN_POINT('Ctrl Pts',(-0.89918504749193,-1.,-1.51805569591479));
#24599=CARTESIAN_POINT('Ctrl Pts',(-0.894452006967538,-1.,-1.50980486807181));
#24600=CARTESIAN_POINT('Ctrl Pts',(-0.892032620296855,-1.,-1.5055822144029));
#24601=CARTESIAN_POINT('',(-0.693717979106305,-1.,-1.60662857109684));
#24602=CARTESIAN_POINT('Origin',(0.,-1.,0.));
#24603=CARTESIAN_POINT('',(-0.745574324794401,-1.,-2.0698113262342));
#24604=CARTESIAN_POINT('Ctrl Pts',(-0.693717979106305,-1.,-1.60662857109684));
#24605=CARTESIAN_POINT('Ctrl Pts',(-0.69571209787897,-1.,-1.61106790957619));
#24606=CARTESIAN_POINT('Ctrl Pts',(-0.699605146398837,-1.,-1.61974673471117));
#24607=CARTESIAN_POINT('Ctrl Pts',(-0.705159151977294,-1.,-1.6321654166204));
#24608=CARTESIAN_POINT('Ctrl Pts',(-0.711993139340447,-1.,-1.64752408828442));
#24609=CARTESIAN_POINT('Ctrl Pts',(-0.71958543378795,-1.,-1.66472880551777));
#24610=CARTESIAN_POINT('Ctrl Pts',(-0.726235967982445,-1.,-1.67996158451922));
#24611=CARTESIAN_POINT('Ctrl Pts',(-0.731963238685357,-1.,-1.69326921972915));
#24612=CARTESIAN_POINT('Ctrl Pts',(-0.736799665716932,-1.,-1.70473309004249));
#24613=CARTESIAN_POINT('Ctrl Pts',(-0.74079516202821,-1.,-1.71447789751001));
#24614=CARTESIAN_POINT('Ctrl Pts',(-0.744021445433093,-1.,-1.72268229916769));
#24615=CARTESIAN_POINT('Ctrl Pts',(-0.746574710097752,-1.,-1.72958533647714));
#24616=CARTESIAN_POINT('Ctrl Pts',(-0.74858246295687,-1.,-1.7355035168033));
#24617=CARTESIAN_POINT('Ctrl Pts',(-0.750193435981249,-1.,-1.74080458267114));
#24618=CARTESIAN_POINT('Ctrl Pts',(-0.751555614164482,-1.,-1.74585086852502));
#24619=CARTESIAN_POINT('Ctrl Pts',(-0.752797683531314,-1.,-1.75095139468794));
#24620=CARTESIAN_POINT('Ctrl Pts',(-0.754009254027829,-1.,-1.75631083600019));
#24621=CARTESIAN_POINT('Ctrl Pts',(-0.755220979974461,-1.,-1.76197817240128));
#24622=CARTESIAN_POINT('Ctrl Pts',(-0.75642189602781,-1.,-1.76789396002998));
#24623=CARTESIAN_POINT('Ctrl Pts',(-0.757578264077029,-1.,-1.77394167108292));
#24624=CARTESIAN_POINT('Ctrl Pts',(-0.758650626677518,-1.,-1.77999411220945));
#24625=CARTESIAN_POINT('Ctrl Pts',(-0.759614401110189,-1.,-1.78596964884604));
#24626=CARTESIAN_POINT('Ctrl Pts',(-0.760469555880749,-1.,-1.7918581561088));
#24627=CARTESIAN_POINT('Ctrl Pts',(-0.761229695230558,-1.,-1.79768986997783));
#24628=CARTESIAN_POINT('Ctrl Pts',(-0.761915336443547,-1.,-1.80351583877342));
#24629=CARTESIAN_POINT('Ctrl Pts',(-0.762546129463938,-1.,-1.80938551463965));
#24630=CARTESIAN_POINT('Ctrl Pts',(-0.763132003836634,-1.,-1.8153211840553));
#24631=CARTESIAN_POINT('Ctrl Pts',(-0.763673465462726,-1.,-1.82131873145266));
#24632=CARTESIAN_POINT('Ctrl Pts',(-0.764165902605995,-1.,-1.82735991200065));
#24633=CARTESIAN_POINT('Ctrl Pts',(-0.764602549687853,-1.,-1.83342077227142));
#24634=CARTESIAN_POINT('Ctrl Pts',(-0.764978057881737,-1.,-1.83948181064835));
#24635=CARTESIAN_POINT('Ctrl Pts',(-0.765291664862029,-1.,-1.84553698875924));
#24636=CARTESIAN_POINT('Ctrl Pts',(-0.765545710619062,-1.,-1.85158945130063));
#24637=CARTESIAN_POINT('Ctrl Pts',(-0.765744212909318,-1.,-1.85764741390394));
#24638=CARTESIAN_POINT('Ctrl Pts',(-0.765891519092547,-1.,-1.86372027063312));
#24639=CARTESIAN_POINT('Ctrl Pts',(-0.765990708546091,-1.,-1.86981398314341));
#24640=CARTESIAN_POINT('Ctrl Pts',(-0.766042837036744,-1.,-1.87592888967883));
#24641=CARTESIAN_POINT('Ctrl Pts',(-0.766047794851865,-1.,-1.88206215302561));
#24642=CARTESIAN_POINT('Ctrl Pts',(-0.766004837062091,-1.,-1.88820926433409));
#24643=CARTESIAN_POINT('Ctrl Pts',(-0.765913193856978,-1.,-1.89436577771388));
#24644=CARTESIAN_POINT('Ctrl Pts',(-0.765772772593386,-1.,-1.90052930393596));
#24645=CARTESIAN_POINT('Ctrl Pts',(-0.765584196937919,-1.,-1.90669961402356));
#24646=CARTESIAN_POINT('Ctrl Pts',(-0.765348465884722,-1.,-1.91287765805169));
#24647=CARTESIAN_POINT('Ctrl Pts',(-0.765066729667088,-1.,-1.91906491634196));
#24648=CARTESIAN_POINT('Ctrl Pts',(-0.764740025488211,-1.,-1.92526263537048));
#24649=CARTESIAN_POINT('Ctrl Pts',(-0.764369010673941,-1.,-1.93147105496382));
#24650=CARTESIAN_POINT('Ctrl Pts',(-0.763954049121458,-1.,-1.93768964875886));
#24651=CARTESIAN_POINT('Ctrl Pts',(-0.763495333538629,-1.,-1.9439174661764));
#24652=CARTESIAN_POINT('Ctrl Pts',(-0.762992990878769,-1.,-1.95015342590024));
#24653=CARTESIAN_POINT('Ctrl Pts',(-0.762447203806179,-1.,-1.95639665309869));
#24654=CARTESIAN_POINT('Ctrl Pts',(-0.761858300014423,-1.,-1.96264672744186));
#24655=CARTESIAN_POINT('Ctrl Pts',(-0.76122669048382,-1.,-1.96890351582499));
#24656=CARTESIAN_POINT('Ctrl Pts',(-0.760552825409757,-1.,-1.97516705321494));
#24657=CARTESIAN_POINT('Ctrl Pts',(-0.75983714745219,-1.,-1.98143741418172));
#24658=CARTESIAN_POINT('Ctrl Pts',(-0.759080037802488,-1.,-1.98771456680874));
#24659=CARTESIAN_POINT('Ctrl Pts',(-0.758281796766761,-1.,-1.99399831098817));
#24660=CARTESIAN_POINT('Ctrl Pts',(-0.757442676862724,-1.,-2.00028834739178));
#24661=CARTESIAN_POINT('Ctrl Pts',(-0.75656290464667,-1.,-2.0065843158773));
#24662=CARTESIAN_POINT('Ctrl Pts',(-0.755642704957865,-1.,-2.01288584328084));
#24663=CARTESIAN_POINT('Ctrl Pts',(-0.754682330722816,-1.,-2.01919259405809));
#24664=CARTESIAN_POINT('Ctrl Pts',(-0.753682061112768,-1.,-2.02550428623313));
#24665=CARTESIAN_POINT('Ctrl Pts',(-0.752642180487211,-1.,-2.03182068456221));
#24666=CARTESIAN_POINT('Ctrl Pts',(-0.751562963361115,-1.,-2.03814160092099));
#24667=CARTESIAN_POINT('Ctrl Pts',(-0.750444657875576,-1.,-2.04446689147979));
#24668=CARTESIAN_POINT('Ctrl Pts',(-0.749287468665046,-1.,-2.05079645592154));
#24669=CARTESIAN_POINT('Ctrl Pts',(-0.748091554183802,-1.,-2.05713023031006));
#24670=CARTESIAN_POINT('Ctrl Pts',(-0.747103932787919,-1.,-2.06220058927826));
#24671=CARTESIAN_POINT('Ctrl Pts',(-0.7463458715442,-1.,-2.06600523016815));
#24672=CARTESIAN_POINT('Ctrl Pts',(-0.745832791378367,-1.,-2.06854248895728));
#24673=CARTESIAN_POINT('Ctrl Pts',(-0.745574324794401,-1.,-2.0698113262342));
#24674=CARTESIAN_POINT('',(-0.61342227326009,-1.,-2.11275013067528));
#24675=CARTESIAN_POINT('',(-0.745574324794401,-1.,-2.0698113262342));
#24676=CARTESIAN_POINT('',(-0.383122945602004,-1.,-1.7075470150345));
#24677=CARTESIAN_POINT('Ctrl Pts',(-0.61342227326009,-1.,-2.11275013067528));
#24678=CARTESIAN_POINT('Ctrl Pts',(-0.6124673655618,-1.,-2.11187554259986));
#24679=CARTESIAN_POINT('Ctrl Pts',(-0.610560911689899,-1.,-2.11012443807238));
#24680=CARTESIAN_POINT('Ctrl Pts',(-0.607711315454876,-1.,-2.1074919961518));
#24681=CARTESIAN_POINT('Ctrl Pts',(-0.60393203073603,-1.,-2.10397049886949));
#24682=CARTESIAN_POINT('Ctrl Pts',(-0.599241616420533,-1.,-2.0995493086477));
#24683=CARTESIAN_POINT('Ctrl Pts',(-0.594585006052162,-1.,-2.0951087622027));
#24684=CARTESIAN_POINT('Ctrl Pts',(-0.589962365403406,-1.,-2.09064881812129));
#24685=CARTESIAN_POINT('Ctrl Pts',(-0.585373918991617,-1.,-2.08616943727951));
#24686=CARTESIAN_POINT('Ctrl Pts',(-0.580819952108063,-1.,-2.08167059018418));
#24687=CARTESIAN_POINT('Ctrl Pts',(-0.576300797416844,-1.,-2.07715226767559));
#24688=CARTESIAN_POINT('Ctrl Pts',(-0.571816823242603,-1.,-2.07261449292824));
#24689=CARTESIAN_POINT('Ctrl Pts',(-0.567368421181087,-1.,-2.06805732997334));
#24690=CARTESIAN_POINT('Ctrl Pts',(-0.562955993082261,-1.,-2.06348090160589));
#24691=CARTESIAN_POINT('Ctrl Pts',(-0.558579940185151,-1.,-2.05888537756462));
#24692=CARTESIAN_POINT('Ctrl Pts',(-0.554240657463906,-1.,-2.05427091604413));
#24693=CARTESIAN_POINT('Ctrl Pts',(-0.549938525150295,-1.,-2.04963761077958));
#24694=CARTESIAN_POINT('Ctrl Pts',(-0.54567390381743,-1.,-2.04498544714588));
#24695=CARTESIAN_POINT('Ctrl Pts',(-0.541447120615659,-1.,-2.04031422690527));
#24696=CARTESIAN_POINT('Ctrl Pts',(-0.537258489833262,-1.,-2.03562362954037));
#24697=CARTESIAN_POINT('Ctrl Pts',(-0.533108355132977,-1.,-2.03091336214426));
#24698=CARTESIAN_POINT('Ctrl Pts',(-0.528997127241914,-1.,-2.0261832908329));
#24699=CARTESIAN_POINT('Ctrl Pts',(-0.524925318333476,-1.,-2.02143356304698));
#24700=CARTESIAN_POINT('Ctrl Pts',(-0.52089359039937,-1.,-2.01666477917286));
#24701=CARTESIAN_POINT('Ctrl Pts',(-0.516902681728687,-1.,-2.01187773939242));
#24702=CARTESIAN_POINT('Ctrl Pts',(-0.512953306961792,-1.,-2.00707309946949));
#24703=CARTESIAN_POINT('Ctrl Pts',(-0.509046069886157,-1.,-2.00225107134734));
#24704=CARTESIAN_POINT('Ctrl Pts',(-0.505181361323026,-1.,-1.99741107463572));
#24705=CARTESIAN_POINT('Ctrl Pts',(-0.501359287727146,-1.,-1.99255149126155));
#24706=CARTESIAN_POINT('Ctrl Pts',(-0.497579909545574,-1.,-1.98767044752932));
#24707=CARTESIAN_POINT('Ctrl Pts',(-0.493843476541495,-1.,-1.98276658761821));
#24708=CARTESIAN_POINT('Ctrl Pts',(-0.490150627860952,-1.,-1.97783973019229));
#24709=CARTESIAN_POINT('Ctrl Pts',(-0.486502692907659,-1.,-1.97289186263272));
#24710=CARTESIAN_POINT('Ctrl Pts',(-0.482901662120691,-1.,-1.96792703422362));
#24711=CARTESIAN_POINT('Ctrl Pts',(-0.479349583074855,-1.,-1.96294933055943));
#24712=CARTESIAN_POINT('Ctrl Pts',(-0.475848034683176,-1.,-1.95796111148177));
#24713=CARTESIAN_POINT('Ctrl Pts',(-0.472397672264072,-1.,-1.95296148278133));
#24714=CARTESIAN_POINT('Ctrl Pts',(-0.468997482913135,-1.,-1.94794381136514));
#24715=CARTESIAN_POINT('Ctrl Pts',(-0.46564546202603,-1.,-1.9428979419619));
#24716=CARTESIAN_POINT('Ctrl Pts',(-0.462340031009056,-1.,-1.93781486640821));
#24717=CARTESIAN_POINT('Ctrl Pts',(-0.459081234547926,-1.,-1.93269066517934));
#24718=CARTESIAN_POINT('Ctrl Pts',(-0.455872005174371,-1.,-1.92753067150476));
#24719=CARTESIAN_POINT('Ctrl Pts',(-0.452719478359432,-1.,-1.92235380648502));
#24720=CARTESIAN_POINT('Ctrl Pts',(-0.449632260106662,-1.,-1.91718342555755));
#24721=CARTESIAN_POINT('Ctrl Pts',(-0.446617343485711,-1.,-1.9120369998112));
#24722=CARTESIAN_POINT('Ctrl Pts',(-0.443677556849151,-1.,-1.90691756144898));
#24723=CARTESIAN_POINT('Ctrl Pts',(-0.440807833704038,-1.,-1.90180124389086));
#24724=CARTESIAN_POINT('Ctrl Pts',(-0.437995003948244,-1.,-1.89663648956466));
#24725=CARTESIAN_POINT('Ctrl Pts',(-0.435225660963383,-1.,-1.89136993975504));
#24726=CARTESIAN_POINT('Ctrl Pts',(-0.432493038548748,-1.,-1.88596913666793));
#24727=CARTESIAN_POINT('Ctrl Pts',(-0.429803062482344,-1.,-1.88044229001832));
#24728=CARTESIAN_POINT('Ctrl Pts',(-0.427183828519102,-1.,-1.87486989291484));
#24729=CARTESIAN_POINT('Ctrl Pts',(-0.424678177291359,-1.,-1.86937803944323));
#24730=CARTESIAN_POINT('Ctrl Pts',(-0.422327307418275,-1.,-1.86408083334028));
#24731=CARTESIAN_POINT('Ctrl Pts',(-0.420157287975619,-1.,-1.85903281096686));
#24732=CARTESIAN_POINT('Ctrl Pts',(-0.418164129143534,-1.,-1.85417632856234));
#24733=CARTESIAN_POINT('Ctrl Pts',(-0.416300022038864,-1.,-1.84929312929882));
#24734=CARTESIAN_POINT('Ctrl Pts',(-0.41448743825434,-1.,-1.8440575707371));
#24735=CARTESIAN_POINT('Ctrl Pts',(-0.412633125322162,-1.,-1.83808953475839));
#24736=CARTESIAN_POINT('Ctrl Pts',(-0.410641256301675,-1.,-1.83100408895216));
#24737=CARTESIAN_POINT('Ctrl Pts',(-0.408428948108533,-1.,-1.8224702267854));
#24738=CARTESIAN_POINT('Ctrl Pts',(-0.405933518411838,-1.,-1.81223801813988));
#24739=CARTESIAN_POINT('Ctrl Pts',(-0.403107976170441,-1.,-1.80012077176221));
#24740=CARTESIAN_POINT('Ctrl Pts',(-0.39991940378308,-1.,-1.78598826347533));
#24741=CARTESIAN_POINT('Ctrl Pts',(-0.39634619612042,-1.,-1.7697556004756));
#24742=CARTESIAN_POINT('Ctrl Pts',(-0.392375812294307,-1.,-1.75137405313962));
#24743=CARTESIAN_POINT('Ctrl Pts',(-0.388877023509191,-1.,-1.7349317097561));
#24744=CARTESIAN_POINT('Ctrl Pts',(-0.38607079032701,-1.,-1.72162022246158));
#24745=CARTESIAN_POINT('Ctrl Pts',(-0.384119047315542,-1.,-1.71231062891958));
#24746=CARTESIAN_POINT('Ctrl Pts',(-0.383122945602004,-1.,-1.7075470150345));
#24747=CARTESIAN_POINT('',(-0.163289472382896,-1.,-1.74236521665491));
#24748=CARTESIAN_POINT('Origin',(0.,-1.,0.));
#24749=CARTESIAN_POINT('',(-0.0694764450219581,-1.,-2.19890268624765));
#24750=CARTESIAN_POINT('Ctrl Pts',(-0.163289472382896,-1.,-1.74236521665491));
#24751=CARTESIAN_POINT('Ctrl Pts',(-0.163814161002002,-1.,-1.7472034950333));
#24752=CARTESIAN_POINT('Ctrl Pts',(-0.164834765707158,-1.,-1.75666056638427));
#24753=CARTESIAN_POINT('Ctrl Pts',(-0.1662793551464,-1.,-1.77018771684844));
#24754=CARTESIAN_POINT('Ctrl Pts',(-0.168032772805197,-1.,-1.7869064998507));
#24755=CARTESIAN_POINT('Ctrl Pts',(-0.169936923904608,-1.,-1.80561530629706));
#24756=CARTESIAN_POINT('Ctrl Pts',(-0.171554770204119,-1.,-1.82215766811545));
#24757=CARTESIAN_POINT('Ctrl Pts',(-0.1728894428919,-1.,-1.83658380527692));
#24758=CARTESIAN_POINT('Ctrl Pts',(-0.173946627587731,-1.,-1.8489811319852));
#24759=CARTESIAN_POINT('Ctrl Pts',(-0.17473525927603,-1.,-1.85948367088837));
#24760=CARTESIAN_POINT('Ctrl Pts',(-0.175268337590758,-1.,-1.86828349694799));
#24761=CARTESIAN_POINT('Ctrl Pts',(-0.175563480746485,-1.,-1.87563767773588));
#24762=CARTESIAN_POINT('Ctrl Pts',(-0.175644148889699,-1.,-1.88188663145367));
#24763=CARTESIAN_POINT('Ctrl Pts',(-0.175538155840648,-1.,-1.88742606273259));
#24764=CARTESIAN_POINT('Ctrl Pts',(-0.175274276190844,-1.,-1.892646301985));
#24765=CARTESIAN_POINT('Ctrl Pts',(-0.174879405091263,-1.,-1.89788101117132));
#24766=CARTESIAN_POINT('Ctrl Pts',(-0.174375518661085,-1.,-1.90335253862834));
#24767=CARTESIAN_POINT('Ctrl Pts',(-0.173776635257817,-1.,-1.90911693975267));
#24768=CARTESIAN_POINT('Ctrl Pts',(-0.173090695383496,-1.,-1.91511429159527));
#24769=CARTESIAN_POINT('Ctrl Pts',(-0.172321621259514,-1.,-1.9212233439798));
#24770=CARTESIAN_POINT('Ctrl Pts',(-0.171471191532988,-1.,-1.92731093582036));
#24771=CARTESIAN_POINT('Ctrl Pts',(-0.170541253116202,-1.,-1.93329183155539));
#24772=CARTESIAN_POINT('Ctrl Pts',(-0.169534904817491,-1.,-1.93915639211581));
#24773=CARTESIAN_POINT('Ctrl Pts',(-0.168455741607556,-1.,-1.94493757756931));
#24774=CARTESIAN_POINT('Ctrl Pts',(-0.167307501784475,-1.,-1.95069027794294));
#24775=CARTESIAN_POINT('Ctrl Pts',(-0.166093592002812,-1.,-1.9564675971873));
#24776=CARTESIAN_POINT('Ctrl Pts',(-0.164816568920269,-1.,-1.96229379940136));
#24777=CARTESIAN_POINT('Ctrl Pts',(-0.163478185457734,-1.,-1.96816512677967));
#24778=CARTESIAN_POINT('Ctrl Pts',(-0.162079693556289,-1.,-1.97406280235188));
#24779=CARTESIAN_POINT('Ctrl Pts',(-0.160622060784611,-1.,-1.97996195437559));
#24780=CARTESIAN_POINT('Ctrl Pts',(-0.159106226437299,-1.,-1.98584238283292));
#24781=CARTESIAN_POINT('Ctrl Pts',(-0.157533331459227,-1.,-1.99169810931908));
#24782=CARTESIAN_POINT('Ctrl Pts',(-0.155904629548783,-1.,-1.99753284771497));
#24783=CARTESIAN_POINT('Ctrl Pts',(-0.154221403049722,-1.,-2.00335565310543));
#24784=CARTESIAN_POINT('Ctrl Pts',(-0.15248488362145,-1.,-2.00917680318424));
#24785=CARTESIAN_POINT('Ctrl Pts',(-0.150696157673078,-1.,-2.01500291940238));
#24786=CARTESIAN_POINT('Ctrl Pts',(-0.148856124775337,-1.,-2.02083464969894));
#24787=CARTESIAN_POINT('Ctrl Pts',(-0.146965557332583,-1.,-2.02666926182017));
#24788=CARTESIAN_POINT('Ctrl Pts',(-0.145025140186057,-1.,-2.03250223739942));
#24789=CARTESIAN_POINT('Ctrl Pts',(-0.143035515058209,-1.,-2.03832911025912));
#24790=CARTESIAN_POINT('Ctrl Pts',(-0.140997332152546,-1.,-2.04414757947916));
#24791=CARTESIAN_POINT('Ctrl Pts',(-0.138911255368966,-1.,-2.04995762001328));
#24792=CARTESIAN_POINT('Ctrl Pts',(-0.136777941218044,-1.,-2.05576044414264));
#24793=CARTESIAN_POINT('Ctrl Pts',(-0.134598026192106,-1.,-2.06155781517842));
#24794=CARTESIAN_POINT('Ctrl Pts',(-0.13237211154771,-1.,-2.06735123910326));
#24795=CARTESIAN_POINT('Ctrl Pts',(-0.130100748328403,-1.,-2.07314114713063));
#24796=CARTESIAN_POINT('Ctrl Pts',(-0.12778444527612,-1.,-2.07892715110987));
#24797=CARTESIAN_POINT('Ctrl Pts',(-0.125423679412061,-1.,-2.08470840653643));
#24798=CARTESIAN_POINT('Ctrl Pts',(-0.123018905621083,-1.,-2.09048392424825));
#24799=CARTESIAN_POINT('Ctrl Pts',(-0.120570567965122,-1.,-2.0962529286773));
#24800=CARTESIAN_POINT('Ctrl Pts',(-0.118079107988355,-1.,-2.102015121329));
#24801=CARTESIAN_POINT('Ctrl Pts',(-0.115544957687926,-1.,-2.10777050261309));
#24802=CARTESIAN_POINT('Ctrl Pts',(-0.112968534419737,-1.,-2.11351924490306));
#24803=CARTESIAN_POINT('Ctrl Pts',(-0.110350236135025,-1.,-2.11926155590865));
#24804=CARTESIAN_POINT('Ctrl Pts',(-0.10769043523109,-1.,-2.12499752307));
#24805=CARTESIAN_POINT('Ctrl Pts',(-0.104989479152739,-1.,-2.13072704887293));
#24806=CARTESIAN_POINT('Ctrl Pts',(-0.1022477005561,-1.,-2.13644992667165));
#24807=CARTESIAN_POINT('Ctrl Pts',(-0.0994654261990915,-1.,-2.14216588396025));
#24808=CARTESIAN_POINT('Ctrl Pts',(-0.0966429852305459,-1.,-2.14787463531795));
#24809=CARTESIAN_POINT('Ctrl Pts',(-0.0937807218867643,-1.,-2.1535759397817));
#24810=CARTESIAN_POINT('Ctrl Pts',(-0.0908789888107265,-1.,-2.15926961544516));
#24811=CARTESIAN_POINT('Ctrl Pts',(-0.0879381291386923,-1.,-2.16495552645014));
#24812=CARTESIAN_POINT('Ctrl Pts',(-0.0849584620835372,-1.,-2.17063357870952));
#24813=CARTESIAN_POINT('Ctrl Pts',(-0.0819402680872765,-1.,-2.176303712113));
#24814=CARTESIAN_POINT('Ctrl Pts',(-0.0788837727685243,-1.,-2.18196589448887));
#24815=CARTESIAN_POINT('Ctrl Pts',(-0.0757891465836148,-1.,-2.1876201139953));
#24816=CARTESIAN_POINT('Ctrl Pts',(-0.0732830357306725,-1.,-2.19213712013662));
#24817=CARTESIAN_POINT('Ctrl Pts',(-0.0713863779526154,-1.,-2.19552129484002));
#24818=CARTESIAN_POINT('Ctrl Pts',(-0.070114353632549,-1.,-2.19777582085423));
#24819=CARTESIAN_POINT('Ctrl Pts',(-0.0694764450219581,-1.,-2.19890268624765));
#24820=CARTESIAN_POINT('',(0.0694764450219584,-1.,-2.19890268624765));
#24821=CARTESIAN_POINT('',(-0.0694764450219581,-1.,-2.19890268624765));
#24822=CARTESIAN_POINT('',(0.163289472382896,-1.,-1.74236521665491));
#24823=CARTESIAN_POINT('Ctrl Pts',(0.0694764450219584,-1.,-2.19890268624765));
#24824=CARTESIAN_POINT('Ctrl Pts',(0.0701143536324926,-1.,-2.19777582085261));
#24825=CARTESIAN_POINT('Ctrl Pts',(0.0713863779524627,-1.,-2.19552129483562));
#24826=CARTESIAN_POINT('Ctrl Pts',(0.0732830357304276,-1.,-2.19213712012956));
#24827=CARTESIAN_POINT('Ctrl Pts',(0.0757891465833411,-1.,-2.1876201139874));
#24828=CARTESIAN_POINT('Ctrl Pts',(0.0788837727683228,-1.,-2.18196589448304));
#24829=CARTESIAN_POINT('Ctrl Pts',(0.0819402680871939,-1.,-2.1763037121106));
#24830=CARTESIAN_POINT('Ctrl Pts',(0.0849584620835643,-1.,-2.17063357871031));
#24831=CARTESIAN_POINT('Ctrl Pts',(0.0879381291387823,-1.,-2.16495552645275));
#24832=CARTESIAN_POINT('Ctrl Pts',(0.0908789888108266,-1.,-2.15926961544808));
#24833=CARTESIAN_POINT('Ctrl Pts',(0.0937807218868345,-1.,-2.15357593978377));
#24834=CARTESIAN_POINT('Ctrl Pts',(0.0966429852305689,-1.,-2.14787463531864));
#24835=CARTESIAN_POINT('Ctrl Pts',(0.0994654261990743,-1.,-2.14216588395974));
#24836=CARTESIAN_POINT('Ctrl Pts',(0.102247700556064,-1.,-2.13644992667052));
#24837=CARTESIAN_POINT('Ctrl Pts',(0.104989479152703,-1.,-2.1307270488718));
#24838=CARTESIAN_POINT('Ctrl Pts',(0.107690435231068,-1.,-2.12499752306927));
#24839=CARTESIAN_POINT('Ctrl Pts',(0.11035023613502,-1.,-2.11926155590849));
#24840=CARTESIAN_POINT('Ctrl Pts',(0.112968534419746,-1.,-2.11351924490335));
#24841=CARTESIAN_POINT('Ctrl Pts',(0.11554495768794,-1.,-2.10777050261359));
#24842=CARTESIAN_POINT('Ctrl Pts',(0.118079107988368,-1.,-2.10201512132945));
#24843=CARTESIAN_POINT('Ctrl Pts',(0.120570567965129,-1.,-2.09625292867756));
#24844=CARTESIAN_POINT('Ctrl Pts',(0.123018905621083,-1.,-2.09048392424826));
#24845=CARTESIAN_POINT('Ctrl Pts',(0.125423679412058,-1.,-2.08470840653628));
#24846=CARTESIAN_POINT('Ctrl Pts',(0.127784445276116,-1.,-2.07892715110967));
#24847=CARTESIAN_POINT('Ctrl Pts',(0.1301007483284,-1.,-2.07314114713047));
#24848=CARTESIAN_POINT('Ctrl Pts',(0.13237211154771,-1.,-2.06735123910319));
#24849=CARTESIAN_POINT('Ctrl Pts',(0.134598026192107,-1.,-2.06155781517844));
#24850=CARTESIAN_POINT('Ctrl Pts',(0.136777941218044,-1.,-2.0557604441427));
#24851=CARTESIAN_POINT('Ctrl Pts',(0.138911255368966,-1.,-2.04995762001333));
#24852=CARTESIAN_POINT('Ctrl Pts',(0.140997332152545,-1.,-2.04414757947919));
#24853=CARTESIAN_POINT('Ctrl Pts',(0.143035515058208,-1.,-2.03832911025913));
#24854=CARTESIAN_POINT('Ctrl Pts',(0.145025140186058,-1.,-2.03250223739941));
#24855=CARTESIAN_POINT('Ctrl Pts',(0.146965557332586,-1.,-2.02666926182017));
#24856=CARTESIAN_POINT('Ctrl Pts',(0.148856124775343,-1.,-2.02083464969897));
#24857=CARTESIAN_POINT('Ctrl Pts',(0.150696157673084,-1.,-2.01500291940243));
#24858=CARTESIAN_POINT('Ctrl Pts',(0.152484883621452,-1.,-2.00917680318426));
#24859=CARTESIAN_POINT('Ctrl Pts',(0.154221403049719,-1.,-2.00335565310539));
#24860=CARTESIAN_POINT('Ctrl Pts',(0.155904629548774,-1.,-1.99753284771487));
#24861=CARTESIAN_POINT('Ctrl Pts',(0.157533331459215,-1.,-1.99169810931893));
#24862=CARTESIAN_POINT('Ctrl Pts',(0.159106226437288,-1.,-1.98584238283279));
#24863=CARTESIAN_POINT('Ctrl Pts',(0.16062206078461,-1.,-1.97996195437557));
#24864=CARTESIAN_POINT('Ctrl Pts',(0.162079693556302,-1.,-1.97406280235204));
#24865=CARTESIAN_POINT('Ctrl Pts',(0.16347818545776,-1.,-1.96816512678));
#24866=CARTESIAN_POINT('Ctrl Pts',(0.1648165689203,-1.,-1.96229379940174));
#24867=CARTESIAN_POINT('Ctrl Pts',(0.166093592002833,-1.,-1.95646759718755));
#24868=CARTESIAN_POINT('Ctrl Pts',(0.167307501784469,-1.,-1.95069027794286));
#24869=CARTESIAN_POINT('Ctrl Pts',(0.168455741607516,-1.,-1.94493757756879));
#24870=CARTESIAN_POINT('Ctrl Pts',(0.169534904817425,-1.,-1.93915639211497));
#24871=CARTESIAN_POINT('Ctrl Pts',(0.170541253116136,-1.,-1.93329183155455));
#24872=CARTESIAN_POINT('Ctrl Pts',(0.17147119153296,-1.,-1.92731093582));
#24873=CARTESIAN_POINT('Ctrl Pts',(0.172321621259557,-1.,-1.92122334398034));
#24874=CARTESIAN_POINT('Ctrl Pts',(0.173090695383619,-1.,-1.91511429159681));
#24875=CARTESIAN_POINT('Ctrl Pts',(0.173776635257984,-1.,-1.90911693975475));
#24876=CARTESIAN_POINT('Ctrl Pts',(0.174375518661222,-1.,-1.90335253863003));
#24877=CARTESIAN_POINT('Ctrl Pts',(0.174879405091277,-1.,-1.89788101117148));
#24878=CARTESIAN_POINT('Ctrl Pts',(0.175274276190664,-1.,-1.89264630198279));
#24879=CARTESIAN_POINT('Ctrl Pts',(0.175538155840286,-1.,-1.88742606272818));
#24880=CARTESIAN_POINT('Ctrl Pts',(0.175644148889271,-1.,-1.88188663144846));
#24881=CARTESIAN_POINT('Ctrl Pts',(0.175563480746205,-1.,-1.87563767773249));
#24882=CARTESIAN_POINT('Ctrl Pts',(0.175268337590901,-1.,-1.86828349694972));
#24883=CARTESIAN_POINT('Ctrl Pts',(0.174735259276856,-1.,-1.85948367089838));
#24884=CARTESIAN_POINT('Ctrl Pts',(0.173946627589401,-1.,-1.84898113200543));
#24885=CARTESIAN_POINT('Ctrl Pts',(0.17288944289442,-1.,-1.83658380530747));
#24886=CARTESIAN_POINT('Ctrl Pts',(0.171554770207306,-1.,-1.82215766815414));
#24887=CARTESIAN_POINT('Ctrl Pts',(0.169936923908078,-1.,-1.80561530633924));
#24888=CARTESIAN_POINT('Ctrl Pts',(0.16803277280837,-1.,-1.78690649988931));
#24889=CARTESIAN_POINT('Ctrl Pts',(0.166279355148738,-1.,-1.77018771687692));
#24890=CARTESIAN_POINT('Ctrl Pts',(0.164834765708484,-1.,-1.75666056640041));
#24891=CARTESIAN_POINT('Ctrl Pts',(0.163814161002474,-1.,-1.74720349503904));
#24892=CARTESIAN_POINT('Ctrl Pts',(0.163289472382896,-1.,-1.74236521665491));
#24893=CARTESIAN_POINT('',(0.383122945602004,-1.,-1.7075470150345));
#24894=CARTESIAN_POINT('Origin',(0.,-1.,0.));
#24895=CARTESIAN_POINT('',(0.61342227326009,-1.,-2.11275013067528));
#24896=CARTESIAN_POINT('Ctrl Pts',(0.383122945602004,-1.,-1.7075470150345));
#24897=CARTESIAN_POINT('Ctrl Pts',(0.384119047314215,-1.,-1.71231062891398));
#24898=CARTESIAN_POINT('Ctrl Pts',(0.386070790323281,-1.,-1.72162022244582));
#24899=CARTESIAN_POINT('Ctrl Pts',(0.388877023502615,-1.,-1.73493170972829));
#24900=CARTESIAN_POINT('Ctrl Pts',(0.392375812285395,-1.,-1.75137405310193));
#24901=CARTESIAN_POINT('Ctrl Pts',(0.396346196110688,-1.,-1.76975560043442));
#24902=CARTESIAN_POINT('Ctrl Pts',(0.399919403774155,-1.,-1.78598826343754));
#24903=CARTESIAN_POINT('Ctrl Pts',(0.403107976163396,-1.,-1.80012077173238));
#24904=CARTESIAN_POINT('Ctrl Pts',(0.405933518407175,-1.,-1.81223801812013));
#24905=CARTESIAN_POINT('Ctrl Pts',(0.408428948106227,-1.,-1.82247022677562));
#24906=CARTESIAN_POINT('Ctrl Pts',(0.410641256301276,-1.,-1.83100408895047));
#24907=CARTESIAN_POINT('Ctrl Pts',(0.412633125322945,-1.,-1.8380895347617));
#24908=CARTESIAN_POINT('Ctrl Pts',(0.414487438255542,-1.,-1.84405757074218));
#24909=CARTESIAN_POINT('Ctrl Pts',(0.416300022039885,-1.,-1.84929312930314));
#24910=CARTESIAN_POINT('Ctrl Pts',(0.418164129144045,-1.,-1.8541763285645));
#24911=CARTESIAN_POINT('Ctrl Pts',(0.420157287975583,-1.,-1.8590328109667));
#24912=CARTESIAN_POINT('Ctrl Pts',(0.422327307417884,-1.,-1.86408083333863));
#24913=CARTESIAN_POINT('Ctrl Pts',(0.424678177290876,-1.,-1.8693780394412));
#24914=CARTESIAN_POINT('Ctrl Pts',(0.427183828518743,-1.,-1.87486989291334));
#24915=CARTESIAN_POINT('Ctrl Pts',(0.429803062482217,-1.,-1.88044229001779));
#24916=CARTESIAN_POINT('Ctrl Pts',(0.432493038548833,-1.,-1.88596913666828));
#24917=CARTESIAN_POINT('Ctrl Pts',(0.43522566096358,-1.,-1.89136993975585));
#24918=CARTESIAN_POINT('Ctrl Pts',(0.437995003948443,-1.,-1.89663648956549));
#24919=CARTESIAN_POINT('Ctrl Pts',(0.44080783370416,-1.,-1.90180124389137));
#24920=CARTESIAN_POINT('Ctrl Pts',(0.44367755684917,-1.,-1.90691756144906));
#24921=CARTESIAN_POINT('Ctrl Pts',(0.446617343485651,-1.,-1.91203699981095));
#24922=CARTESIAN_POINT('Ctrl Pts',(0.449632260106572,-1.,-1.91718342555717));
#24923=CARTESIAN_POINT('Ctrl Pts',(0.452719478359356,-1.,-1.9223538064847));
#24924=CARTESIAN_POINT('Ctrl Pts',(0.455872005174335,-1.,-1.92753067150461));
#24925=CARTESIAN_POINT('Ctrl Pts',(0.459081234547931,-1.,-1.93269066517936));
#24926=CARTESIAN_POINT('Ctrl Pts',(0.462340031009087,-1.,-1.93781486640834));
#24927=CARTESIAN_POINT('Ctrl Pts',(0.465645462026064,-1.,-1.94289794196205));
#24928=CARTESIAN_POINT('Ctrl Pts',(0.468997482913158,-1.,-1.94794381136524));
#24929=CARTESIAN_POINT('Ctrl Pts',(0.472397672264079,-1.,-1.95296148278136));
#24930=CARTESIAN_POINT('Ctrl Pts',(0.475848034683171,-1.,-1.95796111148175));
#24931=CARTESIAN_POINT('Ctrl Pts',(0.479349583074846,-1.,-1.96294933055938));
#24932=CARTESIAN_POINT('Ctrl Pts',(0.482901662120686,-1.,-1.96792703422358));
#24933=CARTESIAN_POINT('Ctrl Pts',(0.486502692907661,-1.,-1.97289186263272));
#24934=CARTESIAN_POINT('Ctrl Pts',(0.490150627860955,-1.,-1.97783973019229));
#24935=CARTESIAN_POINT('Ctrl Pts',(0.493843476541492,-1.,-1.9827665876182));
#24936=CARTESIAN_POINT('Ctrl Pts',(0.497579909545564,-1.,-1.98767044752929));
#24937=CARTESIAN_POINT('Ctrl Pts',(0.501359287727129,-1.,-1.9925514912615));
#24938=CARTESIAN_POINT('Ctrl Pts',(0.505181361323011,-1.,-1.99741107463567));
#24939=CARTESIAN_POINT('Ctrl Pts',(0.509046069886152,-1.,-2.00225107134733));
#24940=CARTESIAN_POINT('Ctrl Pts',(0.512953306961813,-1.,-2.00707309946955));
#24941=CARTESIAN_POINT('Ctrl Pts',(0.516902681728733,-1.,-2.01187773939257));
#24942=CARTESIAN_POINT('Ctrl Pts',(0.520893590399428,-1.,-2.01666477917306));
#24943=CARTESIAN_POINT('Ctrl Pts',(0.524925318333518,-1.,-2.02143356304712));
#24944=CARTESIAN_POINT('Ctrl Pts',(0.52899712724191,-1.,-2.02618329083289));
#24945=CARTESIAN_POINT('Ctrl Pts',(0.533108355132905,-1.,-2.03091336214401));
#24946=CARTESIAN_POINT('Ctrl Pts',(0.537258489833134,-1.,-2.03562362953993));
#24947=CARTESIAN_POINT('Ctrl Pts',(0.54144712061552,-1.,-2.0403142269048));
#24948=CARTESIAN_POINT('Ctrl Pts',(0.545673903817348,-1.,-2.0449854471456));
#24949=CARTESIAN_POINT('Ctrl Pts',(0.549938525150342,-1.,-2.04963761077974));
#24950=CARTESIAN_POINT('Ctrl Pts',(0.554240657464109,-1.,-2.05427091604482));
#24951=CARTESIAN_POINT('Ctrl Pts',(0.558579940185467,-1.,-2.05888537756571));
#24952=CARTESIAN_POINT('Ctrl Pts',(0.562955993082574,-1.,-2.06348090160697));
#24953=CARTESIAN_POINT('Ctrl Pts',(0.567368421181229,-1.,-2.06805732997383));
#24954=CARTESIAN_POINT('Ctrl Pts',(0.571816823242411,-1.,-2.07261449292758));
#24955=CARTESIAN_POINT('Ctrl Pts',(0.576300797416274,-1.,-2.07715226767361));
#24956=CARTESIAN_POINT('Ctrl Pts',(0.580819952107256,-1.,-2.08167059018138));
#24957=CARTESIAN_POINT('Ctrl Pts',(0.585373918990895,-1.,-2.086169437277));
#24958=CARTESIAN_POINT('Ctrl Pts',(0.589962365403189,-1.,-2.09064881812053));
#24959=CARTESIAN_POINT('Ctrl Pts',(0.594585006052823,-1.,-2.09510876220501));
#24960=CARTESIAN_POINT('Ctrl Pts',(0.599241616422144,-1.,-2.09954930865331));
#24961=CARTESIAN_POINT('Ctrl Pts',(0.603932030738212,-1.,-2.10397049887709));
#24962=CARTESIAN_POINT('Ctrl Pts',(0.607711315456826,-1.,-2.10749199615859));
#24963=CARTESIAN_POINT('Ctrl Pts',(0.610560911691113,-1.,-2.11012443807661));
#24964=CARTESIAN_POINT('Ctrl Pts',(0.61246736556225,-1.,-2.11187554260142));
#24965=CARTESIAN_POINT('Ctrl Pts',(0.61342227326009,-1.,-2.11275013067528));
#24966=CARTESIAN_POINT('',(0.745574324794401,-1.,-2.0698113262342));
#24967=CARTESIAN_POINT('',(0.61342227326009,-1.,-2.11275013067528));
#24968=CARTESIAN_POINT('',(0.693717979106306,-1.,-1.60662857109684));
#24969=CARTESIAN_POINT('Ctrl Pts',(0.745574324794401,-1.,-2.0698113262342));
#24970=CARTESIAN_POINT('Ctrl Pts',(0.74583279137781,-1.,-2.06854248895575));
#24971=CARTESIAN_POINT('Ctrl Pts',(0.746345871542695,-1.,-2.06600523016401));
#24972=CARTESIAN_POINT('Ctrl Pts',(0.747103932785504,-1.,-2.06220058927162));
#24973=CARTESIAN_POINT('Ctrl Pts',(0.748091554181101,-1.,-2.05713023030263));
#24974=CARTESIAN_POINT('Ctrl Pts',(0.749287468663053,-1.,-2.05079645591606));
#24975=CARTESIAN_POINT('Ctrl Pts',(0.750444657874758,-1.,-2.04446689147754));
#24976=CARTESIAN_POINT('Ctrl Pts',(0.751562963361383,-1.,-2.03814160092173));
#24977=CARTESIAN_POINT('Ctrl Pts',(0.752642180488104,-1.,-2.03182068456467));
#24978=CARTESIAN_POINT('Ctrl Pts',(0.753682061113765,-1.,-2.02550428623587));
#24979=CARTESIAN_POINT('Ctrl Pts',(0.75468233072352,-1.,-2.01919259406003));
#24980=CARTESIAN_POINT('Ctrl Pts',(0.7556427049581,-1.,-2.01288584328149));
#24981=CARTESIAN_POINT('Ctrl Pts',(0.756562904646496,-1.,-2.00658431587682));
#24982=CARTESIAN_POINT('Ctrl Pts',(0.757442676862341,-1.,-2.00028834739072));
#24983=CARTESIAN_POINT('Ctrl Pts',(0.758281796766377,-1.,-1.9939983109871));
#24984=CARTESIAN_POINT('Ctrl Pts',(0.759080037802242,-1.,-1.98771456680806));
#24985=CARTESIAN_POINT('Ctrl Pts',(0.759837147452135,-1.,-1.98143741418156));
#24986=CARTESIAN_POINT('Ctrl Pts',(0.760552825409855,-1.,-1.97516705321521));
#24987=CARTESIAN_POINT('Ctrl Pts',(0.761226690483986,-1.,-1.96890351582545));
#24988=CARTESIAN_POINT('Ctrl Pts',(0.761858300014575,-1.,-1.96264672744229));
#24989=CARTESIAN_POINT('Ctrl Pts',(0.762447203806263,-1.,-1.95639665309893));
#24990=CARTESIAN_POINT('Ctrl Pts',(0.762992990878774,-1.,-1.95015342590025));
#24991=CARTESIAN_POINT('Ctrl Pts',(0.76349533353858,-1.,-1.94391746617626));
#24992=CARTESIAN_POINT('Ctrl Pts',(0.763954049121393,-1.,-1.93768964875867));
#24993=CARTESIAN_POINT('Ctrl Pts',(0.764369010673889,-1.,-1.93147105496367));
#24994=CARTESIAN_POINT('Ctrl Pts',(0.764740025488189,-1.,-1.92526263537041));
#24995=CARTESIAN_POINT('Ctrl Pts',(0.765066729667095,-1.,-1.91906491634197));
#24996=CARTESIAN_POINT('Ctrl Pts',(0.765348465884739,-1.,-1.91287765805174));
#24997=CARTESIAN_POINT('Ctrl Pts',(0.765584196937936,-1.,-1.90669961402362));
#24998=CARTESIAN_POINT('Ctrl Pts',(0.765772772593395,-1.,-1.90052930393599));
#24999=CARTESIAN_POINT('Ctrl Pts',(0.765913193856979,-1.,-1.89436577771389));
#25000=CARTESIAN_POINT('Ctrl Pts',(0.76600483706209,-1.,-1.88820926433409));
#25001=CARTESIAN_POINT('Ctrl Pts',(0.766047794851868,-1.,-1.88206215302561));
#25002=CARTESIAN_POINT('Ctrl Pts',(0.766042837036759,-1.,-1.87592888967886));
#25003=CARTESIAN_POINT('Ctrl Pts',(0.765990708546111,-1.,-1.86981398314345));
#25004=CARTESIAN_POINT('Ctrl Pts',(0.765891519092557,-1.,-1.86372027063315));
#25005=CARTESIAN_POINT('Ctrl Pts',(0.765744212909305,-1.,-1.85764741390391));
#25006=CARTESIAN_POINT('Ctrl Pts',(0.765545710619023,-1.,-1.85158945130054));
#25007=CARTESIAN_POINT('Ctrl Pts',(0.765291664861971,-1.,-1.84553698875911));
#25008=CARTESIAN_POINT('Ctrl Pts',(0.764978057881687,-1.,-1.83948181064823));
#25009=CARTESIAN_POINT('Ctrl Pts',(0.764602549687845,-1.,-1.8334207722714));
#25010=CARTESIAN_POINT('Ctrl Pts',(0.764165902606055,-1.,-1.8273599120008));
#25011=CARTESIAN_POINT('Ctrl Pts',(0.763673465462854,-1.,-1.82131873145297));
#25012=CARTESIAN_POINT('Ctrl Pts',(0.763132003836783,-1.,-1.81532118405566));
#25013=CARTESIAN_POINT('Ctrl Pts',(0.762546129464036,-1.,-1.80938551463989));
#25014=CARTESIAN_POINT('Ctrl Pts',(0.761915336443515,-1.,-1.80351583877334));
#25015=CARTESIAN_POINT('Ctrl Pts',(0.761229695230359,-1.,-1.79768986997735));
#25016=CARTESIAN_POINT('Ctrl Pts',(0.760469555880425,-1.,-1.79185815610802));
#25017=CARTESIAN_POINT('Ctrl Pts',(0.759614401109868,-1.,-1.78596964884527));
#25018=CARTESIAN_POINT('Ctrl Pts',(0.75865062667738,-1.,-1.77999411220912));
#25019=CARTESIAN_POINT('Ctrl Pts',(0.757578264077238,-1.,-1.77394167108342));
#25020=CARTESIAN_POINT('Ctrl Pts',(0.756421896028403,-1.,-1.76789396003141));
#25021=CARTESIAN_POINT('Ctrl Pts',(0.755220979975262,-1.,-1.7619781724032));
#25022=CARTESIAN_POINT('Ctrl Pts',(0.75400925402848,-1.,-1.75631083600175));
#25023=CARTESIAN_POINT('Ctrl Pts',(0.752797683531377,-1.,-1.75095139468809));
#25024=CARTESIAN_POINT('Ctrl Pts',(0.751555614163629,-1.,-1.74585086852298));
#25025=CARTESIAN_POINT('Ctrl Pts',(0.75019343597954,-1.,-1.74080458266705));
#25026=CARTESIAN_POINT('Ctrl Pts',(0.748582462954854,-1.,-1.73550351679848));
#25027=CARTESIAN_POINT('Ctrl Pts',(0.746574710096436,-1.,-1.72958533647399));
#25028=CARTESIAN_POINT('Ctrl Pts',(0.744021445433764,-1.,-1.7226822991693));
#25029=CARTESIAN_POINT('Ctrl Pts',(0.740795162032087,-1.,-1.71447789751927));
#25030=CARTESIAN_POINT('Ctrl Pts',(0.736799665724771,-1.,-1.70473309006121));
#25031=CARTESIAN_POINT('Ctrl Pts',(0.731963238697195,-1.,-1.69326921975743));
#25032=CARTESIAN_POINT('Ctrl Pts',(0.726235967997433,-1.,-1.67996158455503));
#25033=CARTESIAN_POINT('Ctrl Pts',(0.719585433804282,-1.,-1.6647288055568));
#25034=CARTESIAN_POINT('Ctrl Pts',(0.711993139355394,-1.,-1.64752408832016));
#25035=CARTESIAN_POINT('Ctrl Pts',(0.705159151988319,-1.,-1.63216541664676));
#25036=CARTESIAN_POINT('Ctrl Pts',(0.699605146405088,-1.,-1.61974673472612));
#25037=CARTESIAN_POINT('Ctrl Pts',(0.695712097881194,-1.,-1.61106790958151));
#25038=CARTESIAN_POINT('Ctrl Pts',(0.693717979106306,-1.,-1.60662857109684));
#25039=CARTESIAN_POINT('',(0.892032620296855,-1.,-1.5055822144029));
#25040=CARTESIAN_POINT('Origin',(0.,-1.,0.));
#25041=CARTESIAN_POINT('',(1.23627494547115,-1.,-1.81978687191668));
#25042=CARTESIAN_POINT('Ctrl Pts',(0.892032620296855,-1.,-1.5055822144029));
#25043=CARTESIAN_POINT('Ctrl Pts',(0.894452006964543,-1.,-1.50980486806688));
#25044=CARTESIAN_POINT('Ctrl Pts',(0.89918504748351,-1.,-1.51805569590094));
#25045=CARTESIAN_POINT('Ctrl Pts',(0.905967409625651,-1.,-1.52984849887993));
#25046=CARTESIAN_POINT('Ctrl Pts',(0.914375919026456,-1.,-1.54440491149498));
#25047=CARTESIAN_POINT('Ctrl Pts',(0.923832188944341,-1.,-1.56065988578893));
#25048=CARTESIAN_POINT('Ctrl Pts',(0.932246680108685,-1.,-1.57499388382243));
#25049=CARTESIAN_POINT('Ctrl Pts',(0.939646377893399,-1.,-1.58744937487176));
#25050=CARTESIAN_POINT('Ctrl Pts',(0.946078063315257,-1.,-1.59810042043673));
#25051=CARTESIAN_POINT('Ctrl Pts',(0.951613284356035,-1.,-1.60706069896936));
#25052=CARTESIAN_POINT('Ctrl Pts',(0.95635442292067,-1.,-1.61449324337085));
#25053=CARTESIAN_POINT('Ctrl Pts',(0.960438326101728,-1.,-1.62061638140221));
#25054=CARTESIAN_POINT('Ctrl Pts',(0.964046107040535,-1.,-1.62571930670187));
#25055=CARTESIAN_POINT('Ctrl Pts',(0.967387853230345,-1.,-1.63013849959462));
#25056=CARTESIAN_POINT('Ctrl Pts',(0.970669715997509,-1.,-1.63420665729798));
#25057=CARTESIAN_POINT('Ctrl Pts',(0.974066058287418,-1.,-1.63820952658144));
#25058=CARTESIAN_POINT('Ctrl Pts',(0.977689794119416,-1.,-1.64233990826687));
#25059=CARTESIAN_POINT('Ctrl Pts',(0.981562530939489,-1.,-1.64665139190656));
#25060=CARTESIAN_POINT('Ctrl Pts',(0.98564262292082,-1.,-1.65110016612638));
#25061=CARTESIAN_POINT('Ctrl Pts',(0.989855627854164,-1.,-1.65559044289699));
#25062=CARTESIAN_POINT('Ctrl Pts',(0.994121836661305,-1.,-1.66001553809947));
#25063=CARTESIAN_POINT('Ctrl Pts',(0.998389654952757,-1.,-1.66430758030376));
#25064=CARTESIAN_POINT('Ctrl Pts',(1.00265091003727,-1.,-1.66846059277303));
#25065=CARTESIAN_POINT('Ctrl Pts',(1.00692206696414,-1.,-1.67250335383293));
#25066=CARTESIAN_POINT('Ctrl Pts',(1.01123236493511,-1.,-1.67648246776464));
#25067=CARTESIAN_POINT('Ctrl Pts',(1.01561026162773,-1.,-1.68044289894798));
#25068=CARTESIAN_POINT('Ctrl Pts',(1.02006795074201,-1.,-1.68440578021706));
#25069=CARTESIAN_POINT('Ctrl Pts',(1.02460180535255,-1.,-1.68836910178447));
#25070=CARTESIAN_POINT('Ctrl Pts',(1.02919977579147,-1.,-1.69231840863458));
#25071=CARTESIAN_POINT('Ctrl Pts',(1.03384646003588,-1.,-1.69623414782771));
#25072=CARTESIAN_POINT('Ctrl Pts',(1.03852922490789,-1.,-1.70010052930962));
#25073=CARTESIAN_POINT('Ctrl Pts',(1.04324363334554,-1.,-1.70391338707982));
#25074=CARTESIAN_POINT('Ctrl Pts',(1.04799085404995,-1.,-1.70767646263649));
#25075=CARTESIAN_POINT('Ctrl Pts',(1.05277517202855,-1.,-1.71139783543989));
#25076=CARTESIAN_POINT('Ctrl Pts',(1.05760163192479,-1.,-1.7150865442702));
#25077=CARTESIAN_POINT('Ctrl Pts',(1.06247324680647,-1.,-1.71874858456904));
#25078=CARTESIAN_POINT('Ctrl Pts',(1.06738966975462,-1.,-1.72238500928453));
#25079=CARTESIAN_POINT('Ctrl Pts',(1.07234866990252,-1.,-1.72599406198488));
#25080=CARTESIAN_POINT('Ctrl Pts',(1.0773470373727,-1.,-1.72957248977424));
#25081=CARTESIAN_POINT('Ctrl Pts',(1.08238162784749,-1.,-1.73311705663407));
#25082=CARTESIAN_POINT('Ctrl Pts',(1.08745056285427,-1.,-1.73662628326091));
#25083=CARTESIAN_POINT('Ctrl Pts',(1.09255329056493,-1.,-1.74010053962247));
#25084=CARTESIAN_POINT('Ctrl Pts',(1.09768999241225,-1.,-1.74354119236208));
#25085=CARTESIAN_POINT('Ctrl Pts',(1.10286118991143,-1.,-1.74695004214923));
#25086=CARTESIAN_POINT('Ctrl Pts',(1.10806728183007,-1.,-1.7503286607592));
#25087=CARTESIAN_POINT('Ctrl Pts',(1.11330807582551,-1.,-1.7536777209463));
#25088=CARTESIAN_POINT('Ctrl Pts',(1.11858293216763,-1.,-1.75699720772105));
#25089=CARTESIAN_POINT('Ctrl Pts',(1.12389096855086,-1.,-1.76028671825096));
#25090=CARTESIAN_POINT('Ctrl Pts',(1.12923123555075,-1.,-1.7635457196617));
#25091=CARTESIAN_POINT('Ctrl Pts',(1.1346029180462,-1.,-1.76677384551862));
#25092=CARTESIAN_POINT('Ctrl Pts',(1.14000548336975,-1.,-1.76997111386769));
#25093=CARTESIAN_POINT('Ctrl Pts',(1.1454385822692,-1.,-1.77313777896194));
#25094=CARTESIAN_POINT('Ctrl Pts',(1.15090197841514,-1.,-1.7762742255701));
#25095=CARTESIAN_POINT('Ctrl Pts',(1.15639547194698,-1.,-1.77938085564275));
#25096=CARTESIAN_POINT('Ctrl Pts',(1.16191881298499,-1.,-1.78245795881009));
#25097=CARTESIAN_POINT('Ctrl Pts',(1.16747166312303,-1.,-1.78550566040443));
#25098=CARTESIAN_POINT('Ctrl Pts',(1.17305363177328,-1.,-1.78852398877617));
#25099=CARTESIAN_POINT('Ctrl Pts',(1.17866429440809,-1.,-1.79151291552689));
#25100=CARTESIAN_POINT('Ctrl Pts',(1.18430321697432,-1.,-1.79447240321515));
#25101=CARTESIAN_POINT('Ctrl Pts',(1.18996997934445,-1.,-1.79740245923478));
#25102=CARTESIAN_POINT('Ctrl Pts',(1.19566418930242,-1.,-1.80030314369879));
#25103=CARTESIAN_POINT('Ctrl Pts',(1.20138548938974,-1.,-1.80317454838603));
#25104=CARTESIAN_POINT('Ctrl Pts',(1.20713356605475,-1.,-1.80601678480707));
#25105=CARTESIAN_POINT('Ctrl Pts',(1.21290815708314,-1.,-1.80882996917129));
#25106=CARTESIAN_POINT('Ctrl Pts',(1.21870906103557,-1.,-1.81161420806656));
#25107=CARTESIAN_POINT('Ctrl Pts',(1.2245361330495,-1.,-1.81436959210434));
#25108=CARTESIAN_POINT('Ctrl Pts',(1.2292186489137,-1.,-1.8165508718364));
#25109=CARTESIAN_POINT('Ctrl Pts',(1.2327422452705,-1.,-1.81817389921279));
#25110=CARTESIAN_POINT('Ctrl Pts',(1.23509651170476,-1.,-1.81925017193666));
#25111=CARTESIAN_POINT('Ctrl Pts',(1.23627494547115,-1.,-1.81978687191668));
#25112=CARTESIAN_POINT('',(1.34869019493419,-1.,-1.73811241238545));
#25113=CARTESIAN_POINT('',(1.23627494547115,-1.,-1.81978687191668));
#25114=CARTESIAN_POINT('',(1.15624053661742,-1.,-1.31362392696032));
#25115=CARTESIAN_POINT('Ctrl Pts',(1.34869019493419,-1.,-1.73811241238545));
#25116=CARTESIAN_POINT('Ctrl Pts',(1.34854391898045,-1.,-1.73682580585691));
#25117=CARTESIAN_POINT('Ctrl Pts',(1.34824783112887,-1.,-1.73425417885907));
#25118=CARTESIAN_POINT('Ctrl Pts',(1.34779309152035,-1.,-1.7304014965394));
#25119=CARTESIAN_POINT('Ctrl Pts',(1.34716554819527,-1.,-1.72527410680674));
#25120=CARTESIAN_POINT('Ctrl Pts',(1.34634568653227,-1.,-1.7188807715049));
#25121=CARTESIAN_POINT('Ctrl Pts',(1.34549029589416,-1.,-1.71250340686822));
#25122=CARTESIAN_POINT('Ctrl Pts',(1.34459924533831,-1.,-1.70614212266738));
#25123=CARTESIAN_POINT('Ctrl Pts',(1.34367237124483,-1.,-1.69979707754427));
#25124=CARTESIAN_POINT('Ctrl Pts',(1.34270948206319,-1.,-1.6934684849687));
#25125=CARTESIAN_POINT('Ctrl Pts',(1.341710374848,-1.,-1.68715660868764));
#25126=CARTESIAN_POINT('Ctrl Pts',(1.34067485185203,-1.,-1.68086176030362));
#25127=CARTESIAN_POINT('Ctrl Pts',(1.3396027347034,-1.,-1.67458429426086));
#25128=CARTESIAN_POINT('Ctrl Pts',(1.33849388654388,-1.,-1.66832460783989));
#25129=CARTESIAN_POINT('Ctrl Pts',(1.33734820885262,-1.,-1.66208312541983));
#25130=CARTESIAN_POINT('Ctrl Pts',(1.33616559745172,-1.,-1.65586025952593));
#25131=CARTESIAN_POINT('Ctrl Pts',(1.33494590467993,-1.,-1.6496563728683));
#25132=CARTESIAN_POINT('Ctrl Pts',(1.33368890676572,-1.,-1.6434717485603));
#25133=CARTESIAN_POINT('Ctrl Pts',(1.33239425103724,-1.,-1.63730653475089));
#25134=CARTESIAN_POINT('Ctrl Pts',(1.33106149345645,-1.,-1.63116079730923));
#25135=CARTESIAN_POINT('Ctrl Pts',(1.3296901950568,-1.,-1.62503464209797));
#25136=CARTESIAN_POINT('Ctrl Pts',(1.32828000610449,-1.,-1.61892832270724));
#25137=CARTESIAN_POINT('Ctrl Pts',(1.32683074483356,-1.,-1.6128423401575));
#25138=CARTESIAN_POINT('Ctrl Pts',(1.32534250785782,-1.,-1.60677758290954));
#25139=CARTESIAN_POINT('Ctrl Pts',(1.32381550858256,-1.,-1.60073511858687));
#25140=CARTESIAN_POINT('Ctrl Pts',(1.32224985747682,-1.,-1.59471591079403));
#25141=CARTESIAN_POINT('Ctrl Pts',(1.32064537110892,-1.,-1.58872057258245));
#25142=CARTESIAN_POINT('Ctrl Pts',(1.31900135021432,-1.,-1.58274907898834));
#25143=CARTESIAN_POINT('Ctrl Pts',(1.31731642317187,-1.,-1.5768005650559));
#25144=CARTESIAN_POINT('Ctrl Pts',(1.31558903860016,-1.,-1.57087397835723));
#25145=CARTESIAN_POINT('Ctrl Pts',(1.31381795281002,-1.,-1.56496872402353));
#25146=CARTESIAN_POINT('Ctrl Pts',(1.31200264341696,-1.,-1.55908521254821));
#25147=CARTESIAN_POINT('Ctrl Pts',(1.31014393684222,-1.,-1.55322568759481));
#25148=CARTESIAN_POINT('Ctrl Pts',(1.30824393907473,-1.,-1.54739413957185));
#25149=CARTESIAN_POINT('Ctrl Pts',(1.30630475189556,-1.,-1.54159462645432));
#25150=CARTESIAN_POINT('Ctrl Pts',(1.30432735639489,-1.,-1.53582981268977));
#25151=CARTESIAN_POINT('Ctrl Pts',(1.30231064395568,-1.,-1.53009970283891));
#25152=CARTESIAN_POINT('Ctrl Pts',(1.30024984366328,-1.,-1.52439957861062));
#25153=CARTESIAN_POINT('Ctrl Pts',(1.29813791800747,-1.,-1.51872184912724));
#25154=CARTESIAN_POINT('Ctrl Pts',(1.29596850710509,-1.,-1.51305994241402));
#25155=CARTESIAN_POINT('Ctrl Pts',(1.29373841372842,-1.,-1.50741159078365));
#25156=CARTESIAN_POINT('Ctrl Pts',(1.29145022885181,-1.,-1.50178230149776));
#25157=CARTESIAN_POINT('Ctrl Pts',(1.28911506584254,-1.,-1.49618896881754));
#25158=CARTESIAN_POINT('Ctrl Pts',(1.2867467611644,-1.,-1.4906522831278));
#25159=CARTESIAN_POINT('Ctrl Pts',(1.28435533880201,-1.,-1.4851881711891));
#25160=CARTESIAN_POINT('Ctrl Pts',(1.28194158939517,-1.,-1.47980070347096));
#25161=CARTESIAN_POINT('Ctrl Pts',(1.2794891824849,-1.,-1.4744717526707));
#25162=CARTESIAN_POINT('Ctrl Pts',(1.27696414831089,-1.,-1.46916035917133));
#25163=CARTESIAN_POINT('Ctrl Pts',(1.27433119897822,-1.,-1.46382431332476));
#25164=CARTESIAN_POINT('Ctrl Pts',(1.27156805265289,-1.,-1.45843906294697));
#25165=CARTESIAN_POINT('Ctrl Pts',(1.2686778680489,-1.,-1.45301422764247));
#25166=CARTESIAN_POINT('Ctrl Pts',(1.26570925118868,-1.,-1.44761985001662));
#25167=CARTESIAN_POINT('Ctrl Pts',(1.26273903323858,-1.,-1.44236470511303));
#25168=CARTESIAN_POINT('Ctrl Pts',(1.25983531012005,-1.,-1.43734919180848));
#25169=CARTESIAN_POINT('Ctrl Pts',(1.25702687965755,-1.,-1.43262645609691));
#25170=CARTESIAN_POINT('Ctrl Pts',(1.25426945222639,-1.,-1.42815938799387));
#25171=CARTESIAN_POINT('Ctrl Pts',(1.2514145557001,-1.,-1.42378102115575));
#25172=CARTESIAN_POINT('Ctrl Pts',(1.24824430986571,-1.,-1.41923722596025));
#25173=CARTESIAN_POINT('Ctrl Pts',(1.24450600513056,-1.,-1.41422913175179));
#25174=CARTESIAN_POINT('Ctrl Pts',(1.23994455029534,-1.,-1.40845295531283));
#25175=CARTESIAN_POINT('Ctrl Pts',(1.23434087290423,-1.,-1.40164708206106));
#25176=CARTESIAN_POINT('Ctrl Pts',(1.22752961899387,-1.,-1.39361389568796));
#25177=CARTESIAN_POINT('Ctrl Pts',(1.21938737280852,-1.,-1.38420564527715));
#25178=CARTESIAN_POINT('Ctrl Pts',(1.20982812925645,-1.,-1.37331915607905));
#25179=CARTESIAN_POINT('Ctrl Pts',(1.1987959077932,-1.,-1.36088705043885));
#25180=CARTESIAN_POINT('Ctrl Pts',(1.18625865667441,-1.,-1.34687054001093));
#25181=CARTESIAN_POINT('Ctrl Pts',(1.17501305789857,-1.,-1.33437539347008));
#25182=CARTESIAN_POINT('Ctrl Pts',(1.16589330093588,-1.,-1.32428080721772));
#25183=CARTESIAN_POINT('Ctrl Pts',(1.15950888730809,-1.,-1.31722977216397));
#25184=CARTESIAN_POINT('Ctrl Pts',(1.15624053661742,-1.,-1.31362392696032));
#25185=CARTESIAN_POINT('',(1.31362392696032,-1.,-1.15624053661742));
#25186=CARTESIAN_POINT('Origin',(0.,-1.,0.));
#25187=CARTESIAN_POINT('',(1.73811241238545,-1.,-1.34869019493419));
#25188=CARTESIAN_POINT('Ctrl Pts',(1.31362392696032,-1.,-1.15624053661742));
#25189=CARTESIAN_POINT('Ctrl Pts',(1.3172297721596,-1.,-1.15950888730433));
#25190=CARTESIAN_POINT('Ctrl Pts',(1.32428080720544,-1.,-1.16589330092532));
#25191=CARTESIAN_POINT('Ctrl Pts',(1.33437539344842,-1.,-1.17501305787994));
#25192=CARTESIAN_POINT('Ctrl Pts',(1.34687053998157,-1.,-1.18625865664915));
#25193=CARTESIAN_POINT('Ctrl Pts',(1.36088705040677,-1.,-1.1987959077656));
#25194=CARTESIAN_POINT('Ctrl Pts',(1.37331915604962,-1.,-1.20982812923113));
#25195=CARTESIAN_POINT('Ctrl Pts',(1.38420564525391,-1.,-1.21938737278853));
#25196=CARTESIAN_POINT('Ctrl Pts',(1.39361389567257,-1.,-1.22752961898063));
#25197=CARTESIAN_POINT('Ctrl Pts',(1.40164708205345,-1.,-1.23434087289768));
#25198=CARTESIAN_POINT('Ctrl Pts',(1.40845295531151,-1.,-1.23994455029421));
#25199=CARTESIAN_POINT('Ctrl Pts',(1.41422913175437,-1.,-1.24450600513278));
#25200=CARTESIAN_POINT('Ctrl Pts',(1.41923722596421,-1.,-1.24824430986911));
#25201=CARTESIAN_POINT('Ctrl Pts',(1.42378102115911,-1.,-1.25141455570299));
#25202=CARTESIAN_POINT('Ctrl Pts',(1.42815938799555,-1.,-1.25426945222783));
#25203=CARTESIAN_POINT('Ctrl Pts',(1.43262645609679,-1.,-1.25702687965744));
#25204=CARTESIAN_POINT('Ctrl Pts',(1.43734919180719,-1.,-1.25983531011894));
#25205=CARTESIAN_POINT('Ctrl Pts',(1.44236470511145,-1.,-1.26273903323723));
#25206=CARTESIAN_POINT('Ctrl Pts',(1.44761985001544,-1.,-1.26570925118767));
#25207=CARTESIAN_POINT('Ctrl Pts',(1.45301422764205,-1.,-1.26867786804854));
#25208=CARTESIAN_POINT('Ctrl Pts',(1.45843906294725,-1.,-1.27156805265312));
#25209=CARTESIAN_POINT('Ctrl Pts',(1.4638243133254,-1.,-1.27433119897877));
#25210=CARTESIAN_POINT('Ctrl Pts',(1.46916035917197,-1.,-1.27696414831144));
#25211=CARTESIAN_POINT('Ctrl Pts',(1.4744717526711,-1.,-1.27948918248524));
#25212=CARTESIAN_POINT('Ctrl Pts',(1.47980070347102,-1.,-1.28194158939522));
#25213=CARTESIAN_POINT('Ctrl Pts',(1.48518817118891,-1.,-1.28435533880184));
#25214=CARTESIAN_POINT('Ctrl Pts',(1.4906522831275,-1.,-1.28674676116415));
#25215=CARTESIAN_POINT('Ctrl Pts',(1.49618896881729,-1.,-1.28911506584232));
#25216=CARTESIAN_POINT('Ctrl Pts',(1.50178230149764,-1.,-1.29145022885171));
#25217=CARTESIAN_POINT('Ctrl Pts',(1.50741159078367,-1.,-1.29373841372843));
#25218=CARTESIAN_POINT('Ctrl Pts',(1.51305994241412,-1.,-1.29596850710518));
#25219=CARTESIAN_POINT('Ctrl Pts',(1.51872184912735,-1.,-1.29813791800757));
#25220=CARTESIAN_POINT('Ctrl Pts',(1.5243995786107,-1.,-1.30024984366334));
#25221=CARTESIAN_POINT('Ctrl Pts',(1.53009970283893,-1.,-1.3023106439557));
#25222=CARTESIAN_POINT('Ctrl Pts',(1.53582981268976,-1.,-1.30432735639487));
#25223=CARTESIAN_POINT('Ctrl Pts',(1.54159462645428,-1.,-1.30630475189553));
#25224=CARTESIAN_POINT('Ctrl Pts',(1.54739413957183,-1.,-1.30824393907471));
#25225=CARTESIAN_POINT('Ctrl Pts',(1.55322568759481,-1.,-1.31014393684221));
#25226=CARTESIAN_POINT('Ctrl Pts',(1.55908521254822,-1.,-1.31200264341696));
#25227=CARTESIAN_POINT('Ctrl Pts',(1.56496872402352,-1.,-1.31381795281002));
#25228=CARTESIAN_POINT('Ctrl Pts',(1.57087397835721,-1.,-1.31558903860015));
#25229=CARTESIAN_POINT('Ctrl Pts',(1.57680056505585,-1.,-1.31731642317183));
#25230=CARTESIAN_POINT('Ctrl Pts',(1.58274907898829,-1.,-1.31900135021428));
#25231=CARTESIAN_POINT('Ctrl Pts',(1.58872057258244,-1.,-1.32064537110891));
#25232=CARTESIAN_POINT('Ctrl Pts',(1.59471591079408,-1.,-1.32224985747686));
#25233=CARTESIAN_POINT('Ctrl Pts',(1.600735118587,-1.,-1.32381550858266));
#25234=CARTESIAN_POINT('Ctrl Pts',(1.6067775829097,-1.,-1.32534250785794));
#25235=CARTESIAN_POINT('Ctrl Pts',(1.61284234015762,-1.,-1.32683074483365));
#25236=CARTESIAN_POINT('Ctrl Pts',(1.61892832270723,-1.,-1.32828000610448));
#25237=CARTESIAN_POINT('Ctrl Pts',(1.62503464209777,-1.,-1.32969019505665));
#25238=CARTESIAN_POINT('Ctrl Pts',(1.63116079730887,-1.,-1.33106149345618));
#25239=CARTESIAN_POINT('Ctrl Pts',(1.63730653475049,-1.,-1.33239425103694));
#25240=CARTESIAN_POINT('Ctrl Pts',(1.64347174856007,-1.,-1.33368890676554));
#25241=CARTESIAN_POINT('Ctrl Pts',(1.64965637286843,-1.,-1.33494590468003));
#25242=CARTESIAN_POINT('Ctrl Pts',(1.65586025952651,-1.,-1.33616559745217));
#25243=CARTESIAN_POINT('Ctrl Pts',(1.66208312542073,-1.,-1.33734820885331));
#25244=CARTESIAN_POINT('Ctrl Pts',(1.66832460784078,-1.,-1.33849388654458));
#25245=CARTESIAN_POINT('Ctrl Pts',(1.67458429426126,-1.,-1.33960273470372));
#25246=CARTESIAN_POINT('Ctrl Pts',(1.68086176030308,-1.,-1.3406748518516));
#25247=CARTESIAN_POINT('Ctrl Pts',(1.68715660868602,-1.,-1.34171037484673));
#25248=CARTESIAN_POINT('Ctrl Pts',(1.6934684849664,-1.,-1.34270948206139));
#25249=CARTESIAN_POINT('Ctrl Pts',(1.69979707754221,-1.,-1.34367237124322));
#25250=CARTESIAN_POINT('Ctrl Pts',(1.70614212266676,-1.,-1.34459924533783));
#25251=CARTESIAN_POINT('Ctrl Pts',(1.71250340687011,-1.,-1.34549029589563));
#25252=CARTESIAN_POINT('Ctrl Pts',(1.7188807715095,-1.,-1.34634568653586));
#25253=CARTESIAN_POINT('Ctrl Pts',(1.72527410681298,-1.,-1.34716554820013));
#25254=CARTESIAN_POINT('Ctrl Pts',(1.73040149654497,-1.,-1.3477930915247));
#25255=CARTESIAN_POINT('Ctrl Pts',(1.73425417886254,-1.,-1.34824783113158));
#25256=CARTESIAN_POINT('Ctrl Pts',(1.73682580585819,-1.,-1.34854391898145));
#25257=CARTESIAN_POINT('Ctrl Pts',(1.73811241238545,-1.,-1.34869019493419));
#25258=CARTESIAN_POINT('',(1.81978687191668,-1.,-1.23627494547115));
#25259=CARTESIAN_POINT('',(1.73811241238545,-1.,-1.34869019493419));
#25260=CARTESIAN_POINT('',(1.5055822144029,-1.,-0.892032620296855));
#25261=CARTESIAN_POINT('Ctrl Pts',(1.81978687191668,-1.,-1.23627494547115));
#25262=CARTESIAN_POINT('Ctrl Pts',(1.81925017193531,-1.,-1.23509651170384));
#25263=CARTESIAN_POINT('Ctrl Pts',(1.81817389920914,-1.,-1.23274224526804));
#25264=CARTESIAN_POINT('Ctrl Pts',(1.81655087183054,-1.,-1.22921864890975));
#25265=CARTESIAN_POINT('Ctrl Pts',(1.81436959209778,-1.,-1.22453613304507));
#25266=CARTESIAN_POINT('Ctrl Pts',(1.81161420806172,-1.,-1.2187090610323));
#25267=CARTESIAN_POINT('Ctrl Pts',(1.80882996916931,-1.,-1.2129081570818));
#25268=CARTESIAN_POINT('Ctrl Pts',(1.80601678480772,-1.,-1.20713356605519));
#25269=CARTESIAN_POINT('Ctrl Pts',(1.8031745483882,-1.,-1.2013854893912));
#25270=CARTESIAN_POINT('Ctrl Pts',(1.80030314370121,-1.,-1.19566418930405));
#25271=CARTESIAN_POINT('Ctrl Pts',(1.79740245923649,-1.,-1.1899699793456));
#25272=CARTESIAN_POINT('Ctrl Pts',(1.79447240321572,-1.,-1.18430321697471));
#25273=CARTESIAN_POINT('Ctrl Pts',(1.79151291552646,-1.,-1.17866429440781));
#25274=CARTESIAN_POINT('Ctrl Pts',(1.78852398877523,-1.,-1.17305363177265));
#25275=CARTESIAN_POINT('Ctrl Pts',(1.78550566040349,-1.,-1.16747166312239));
#25276=CARTESIAN_POINT('Ctrl Pts',(1.78245795880949,-1.,-1.16191881298458));
#25277=CARTESIAN_POINT('Ctrl Pts',(1.77938085564261,-1.,-1.15639547194689));
#25278=CARTESIAN_POINT('Ctrl Pts',(1.77627422557034,-1.,-1.15090197841531));
#25279=CARTESIAN_POINT('Ctrl Pts',(1.77313777896234,-1.,-1.14543858226948));
#25280=CARTESIAN_POINT('Ctrl Pts',(1.76997111386806,-1.,-1.14000548337));
#25281=CARTESIAN_POINT('Ctrl Pts',(1.76677384551883,-1.,-1.13460291804635));
#25282=CARTESIAN_POINT('Ctrl Pts',(1.76354571966171,-1.,-1.12923123555076));
#25283=CARTESIAN_POINT('Ctrl Pts',(1.76028671825084,-1.,-1.12389096855078));
#25284=CARTESIAN_POINT('Ctrl Pts',(1.75699720772089,-1.,-1.11858293216752));
#25285=CARTESIAN_POINT('Ctrl Pts',(1.75367772094617,-1.,-1.11330807582542));
#25286=CARTESIAN_POINT('Ctrl Pts',(1.75032866075914,-1.,-1.10806728183003));
#25287=CARTESIAN_POINT('Ctrl Pts',(1.74695004214924,-1.,-1.10286118991144));
#25288=CARTESIAN_POINT('Ctrl Pts',(1.74354119236212,-1.,-1.09768999241229));
#25289=CARTESIAN_POINT('Ctrl Pts',(1.74010053962252,-1.,-1.09255329056496));
#25290=CARTESIAN_POINT('Ctrl Pts',(1.73662628326093,-1.,-1.08745056285429));
#25291=CARTESIAN_POINT('Ctrl Pts',(1.73311705663407,-1.,-1.08238162784749));
#25292=CARTESIAN_POINT('Ctrl Pts',(1.72957248977424,-1.,-1.0773470373727));
#25293=CARTESIAN_POINT('Ctrl Pts',(1.72599406198489,-1.,-1.07234866990252));
#25294=CARTESIAN_POINT('Ctrl Pts',(1.72238500928456,-1.,-1.06738966975463));
#25295=CARTESIAN_POINT('Ctrl Pts',(1.71874858456908,-1.,-1.0624732468065));
#25296=CARTESIAN_POINT('Ctrl Pts',(1.71508654427022,-1.,-1.05760163192481));
#25297=CARTESIAN_POINT('Ctrl Pts',(1.71139783543986,-1.,-1.05277517202854));
#25298=CARTESIAN_POINT('Ctrl Pts',(1.70767646263641,-1.,-1.0479908540499));
#25299=CARTESIAN_POINT('Ctrl Pts',(1.70391338707969,-1.,-1.04324363334546));
#25300=CARTESIAN_POINT('Ctrl Pts',(1.70010052930951,-1.,-1.03852922490782));
#25301=CARTESIAN_POINT('Ctrl Pts',(1.69623414782769,-1.,-1.03384646003587));
#25302=CARTESIAN_POINT('Ctrl Pts',(1.69231840863471,-1.,-1.02919977579155));
#25303=CARTESIAN_POINT('Ctrl Pts',(1.68836910178475,-1.,-1.02460180535272));
#25304=CARTESIAN_POINT('Ctrl Pts',(1.68440578021739,-1.,-1.02006795074222));
#25305=CARTESIAN_POINT('Ctrl Pts',(1.6804428989482,-1.,-1.01561026162787));
#25306=CARTESIAN_POINT('Ctrl Pts',(1.67648246776457,-1.,-1.01123236493507));
#25307=CARTESIAN_POINT('Ctrl Pts',(1.67250335383248,-1.,-1.00692206696387));
#25308=CARTESIAN_POINT('Ctrl Pts',(1.66846059277231,-1.,-1.00265091003682));
#25309=CARTESIAN_POINT('Ctrl Pts',(1.66430758030304,-1.,-0.998389654952317));
#25310=CARTESIAN_POINT('Ctrl Pts',(1.66001553809916,-1.,-0.994121836661116));
#25311=CARTESIAN_POINT('Ctrl Pts',(1.65559044289746,-1.,-0.98985562785445));
#25312=CARTESIAN_POINT('Ctrl Pts',(1.6511001661277,-1.,-0.985642622921626));
#25313=CARTESIAN_POINT('Ctrl Pts',(1.64665139190834,-1.,-0.981562530940574));
#25314=CARTESIAN_POINT('Ctrl Pts',(1.64233990826831,-1.,-0.977689794120297));
#25315=CARTESIAN_POINT('Ctrl Pts',(1.63820952658157,-1.,-0.974066058287501));
#25316=CARTESIAN_POINT('Ctrl Pts',(1.63420665729609,-1.,-0.970669715996356));
#25317=CARTESIAN_POINT('Ctrl Pts',(1.63013849959083,-1.,-0.967387853228041));
#25318=CARTESIAN_POINT('Ctrl Pts',(1.6257193066974,-1.,-0.964046107037821));
#25319=CARTESIAN_POINT('Ctrl Pts',(1.62061638139929,-1.,-0.960438326099958));
#25320=CARTESIAN_POINT('Ctrl Pts',(1.61449324337233,-1.,-0.956354422921573));
#25321=CARTESIAN_POINT('Ctrl Pts',(1.60706069897794,-1.,-0.951613284361248));
#25322=CARTESIAN_POINT('Ctrl Pts',(1.59810042045408,-1.,-0.946078063325796));
#25323=CARTESIAN_POINT('Ctrl Pts',(1.58744937489796,-1.,-0.939646377909319));
#25324=CARTESIAN_POINT('Ctrl Pts',(1.57499388385561,-1.,-0.932246680128849));
#25325=CARTESIAN_POINT('Ctrl Pts',(1.56065988582509,-1.,-0.923832188966322));
#25326=CARTESIAN_POINT('Ctrl Pts',(1.54440491152807,-1.,-0.91437591904658));
#25327=CARTESIAN_POINT('Ctrl Pts',(1.52984849890434,-1.,-0.905967409640499));
#25328=CARTESIAN_POINT('Ctrl Pts',(1.51805569591479,-1.,-0.89918504749193));
#25329=CARTESIAN_POINT('Ctrl Pts',(1.50980486807181,-1.,-0.894452006967538));
#25330=CARTESIAN_POINT('Ctrl Pts',(1.5055822144029,-1.,-0.892032620296855));
#25331=CARTESIAN_POINT('',(1.60662857109684,-1.,-0.693717979106306));
#25332=CARTESIAN_POINT('Origin',(0.,-1.,0.));
#25333=CARTESIAN_POINT('',(2.0698113262342,-1.,-0.745574324794401));
#25334=CARTESIAN_POINT('Ctrl Pts',(1.60662857109684,-1.,-0.693717979106306));
#25335=CARTESIAN_POINT('Ctrl Pts',(1.61106790957619,-1.,-0.69571209787897));
#25336=CARTESIAN_POINT('Ctrl Pts',(1.61974673471117,-1.,-0.699605146398837));
#25337=CARTESIAN_POINT('Ctrl Pts',(1.6321654166204,-1.,-0.705159151977294));
#25338=CARTESIAN_POINT('Ctrl Pts',(1.64752408828442,-1.,-0.711993139340448));
#25339=CARTESIAN_POINT('Ctrl Pts',(1.66472880551777,-1.,-0.71958543378795));
#25340=CARTESIAN_POINT('Ctrl Pts',(1.67996158451922,-1.,-0.726235967982445));
#25341=CARTESIAN_POINT('Ctrl Pts',(1.69326921972915,-1.,-0.731963238685357));
#25342=CARTESIAN_POINT('Ctrl Pts',(1.70473309004249,-1.,-0.736799665716932));
#25343=CARTESIAN_POINT('Ctrl Pts',(1.71447789751001,-1.,-0.74079516202821));
#25344=CARTESIAN_POINT('Ctrl Pts',(1.72268229916769,-1.,-0.744021445433094));
#25345=CARTESIAN_POINT('Ctrl Pts',(1.72958533647714,-1.,-0.746574710097752));
#25346=CARTESIAN_POINT('Ctrl Pts',(1.7355035168033,-1.,-0.74858246295687));
#25347=CARTESIAN_POINT('Ctrl Pts',(1.74080458267114,-1.,-0.75019343598125));
#25348=CARTESIAN_POINT('Ctrl Pts',(1.74585086852502,-1.,-0.751555614164483));
#25349=CARTESIAN_POINT('Ctrl Pts',(1.75095139468794,-1.,-0.752797683531314));
#25350=CARTESIAN_POINT('Ctrl Pts',(1.75631083600019,-1.,-0.754009254027829));
#25351=CARTESIAN_POINT('Ctrl Pts',(1.76197817240128,-1.,-0.755220979974462));
#25352=CARTESIAN_POINT('Ctrl Pts',(1.76789396002998,-1.,-0.75642189602781));
#25353=CARTESIAN_POINT('Ctrl Pts',(1.77394167108292,-1.,-0.757578264077029));
#25354=CARTESIAN_POINT('Ctrl Pts',(1.77999411220945,-1.,-0.758650626677519));
#25355=CARTESIAN_POINT('Ctrl Pts',(1.78596964884604,-1.,-0.75961440111019));
#25356=CARTESIAN_POINT('Ctrl Pts',(1.7918581561088,-1.,-0.760469555880749));
#25357=CARTESIAN_POINT('Ctrl Pts',(1.79768986997783,-1.,-0.761229695230558));
#25358=CARTESIAN_POINT('Ctrl Pts',(1.80351583877342,-1.,-0.761915336443547));
#25359=CARTESIAN_POINT('Ctrl Pts',(1.80938551463965,-1.,-0.762546129463938));
#25360=CARTESIAN_POINT('Ctrl Pts',(1.8153211840553,-1.,-0.763132003836634));
#25361=CARTESIAN_POINT('Ctrl Pts',(1.82131873145266,-1.,-0.763673465462727));
#25362=CARTESIAN_POINT('Ctrl Pts',(1.82735991200065,-1.,-0.764165902605995));
#25363=CARTESIAN_POINT('Ctrl Pts',(1.83342077227142,-1.,-0.764602549687853));
#25364=CARTESIAN_POINT('Ctrl Pts',(1.83948181064835,-1.,-0.764978057881738));
#25365=CARTESIAN_POINT('Ctrl Pts',(1.84553698875924,-1.,-0.765291664862029));
#25366=CARTESIAN_POINT('Ctrl Pts',(1.85158945130063,-1.,-0.765545710619063));
#25367=CARTESIAN_POINT('Ctrl Pts',(1.85764741390394,-1.,-0.765744212909319));
#25368=CARTESIAN_POINT('Ctrl Pts',(1.86372027063312,-1.,-0.765891519092547));
#25369=CARTESIAN_POINT('Ctrl Pts',(1.86981398314341,-1.,-0.765990708546091));
#25370=CARTESIAN_POINT('Ctrl Pts',(1.87592888967883,-1.,-0.766042837036744));
#25371=CARTESIAN_POINT('Ctrl Pts',(1.88206215302561,-1.,-0.766047794851865));
#25372=CARTESIAN_POINT('Ctrl Pts',(1.88820926433409,-1.,-0.766004837062091));
#25373=CARTESIAN_POINT('Ctrl Pts',(1.89436577771388,-1.,-0.765913193856978));
#25374=CARTESIAN_POINT('Ctrl Pts',(1.90052930393596,-1.,-0.765772772593386));
#25375=CARTESIAN_POINT('Ctrl Pts',(1.90669961402356,-1.,-0.765584196937919));
#25376=CARTESIAN_POINT('Ctrl Pts',(1.91287765805169,-1.,-0.765348465884722));
#25377=CARTESIAN_POINT('Ctrl Pts',(1.91906491634196,-1.,-0.765066729667089));
#25378=CARTESIAN_POINT('Ctrl Pts',(1.92526263537048,-1.,-0.764740025488212));
#25379=CARTESIAN_POINT('Ctrl Pts',(1.93147105496382,-1.,-0.764369010673941));
#25380=CARTESIAN_POINT('Ctrl Pts',(1.93768964875886,-1.,-0.763954049121459));
#25381=CARTESIAN_POINT('Ctrl Pts',(1.9439174661764,-1.,-0.763495333538629));
#25382=CARTESIAN_POINT('Ctrl Pts',(1.95015342590024,-1.,-0.762992990878769));
#25383=CARTESIAN_POINT('Ctrl Pts',(1.95639665309869,-1.,-0.762447203806179));
#25384=CARTESIAN_POINT('Ctrl Pts',(1.96264672744186,-1.,-0.761858300014424));
#25385=CARTESIAN_POINT('Ctrl Pts',(1.96890351582499,-1.,-0.761226690483821));
#25386=CARTESIAN_POINT('Ctrl Pts',(1.97516705321494,-1.,-0.760552825409757));
#25387=CARTESIAN_POINT('Ctrl Pts',(1.98143741418172,-1.,-0.75983714745219));
#25388=CARTESIAN_POINT('Ctrl Pts',(1.98771456680874,-1.,-0.759080037802488));
#25389=CARTESIAN_POINT('Ctrl Pts',(1.99399831098817,-1.,-0.758281796766761));
#25390=CARTESIAN_POINT('Ctrl Pts',(2.00028834739178,-1.,-0.757442676862724));
#25391=CARTESIAN_POINT('Ctrl Pts',(2.0065843158773,-1.,-0.756562904646671));
#25392=CARTESIAN_POINT('Ctrl Pts',(2.01288584328084,-1.,-0.755642704957865));
#25393=CARTESIAN_POINT('Ctrl Pts',(2.01919259405809,-1.,-0.754682330722816));
#25394=CARTESIAN_POINT('Ctrl Pts',(2.02550428623313,-1.,-0.753682061112768));
#25395=CARTESIAN_POINT('Ctrl Pts',(2.03182068456221,-1.,-0.752642180487211));
#25396=CARTESIAN_POINT('Ctrl Pts',(2.03814160092099,-1.,-0.751562963361115));
#25397=CARTESIAN_POINT('Ctrl Pts',(2.04446689147979,-1.,-0.750444657875576));
#25398=CARTESIAN_POINT('Ctrl Pts',(2.05079645592154,-1.,-0.749287468665046));
#25399=CARTESIAN_POINT('Ctrl Pts',(2.05713023031006,-1.,-0.748091554183803));
#25400=CARTESIAN_POINT('Ctrl Pts',(2.06220058927826,-1.,-0.74710393278792));
#25401=CARTESIAN_POINT('Ctrl Pts',(2.06600523016815,-1.,-0.746345871544201));
#25402=CARTESIAN_POINT('Ctrl Pts',(2.06854248895728,-1.,-0.745832791378367));
#25403=CARTESIAN_POINT('Ctrl Pts',(2.0698113262342,-1.,-0.745574324794401));
#25404=CARTESIAN_POINT('',(2.11275013067528,-1.,-0.61342227326009));
#25405=CARTESIAN_POINT('',(2.0698113262342,-1.,-0.745574324794401));
#25406=CARTESIAN_POINT('',(1.7075470150345,-1.,-0.383122945602004));
#25407=CARTESIAN_POINT('Ctrl Pts',(2.11275013067528,-1.,-0.61342227326009));
#25408=CARTESIAN_POINT('Ctrl Pts',(2.11187554259986,-1.,-0.6124673655618));
#25409=CARTESIAN_POINT('Ctrl Pts',(2.11012443807238,-1.,-0.610560911689899));
#25410=CARTESIAN_POINT('Ctrl Pts',(2.1074919961518,-1.,-0.607711315454876));
#25411=CARTESIAN_POINT('Ctrl Pts',(2.10397049886949,-1.,-0.60393203073603));
#25412=CARTESIAN_POINT('Ctrl Pts',(2.0995493086477,-1.,-0.599241616420534));
#25413=CARTESIAN_POINT('Ctrl Pts',(2.0951087622027,-1.,-0.594585006052162));
#25414=CARTESIAN_POINT('Ctrl Pts',(2.09064881812129,-1.,-0.589962365403406));
#25415=CARTESIAN_POINT('Ctrl Pts',(2.08616943727951,-1.,-0.585373918991617));
#25416=CARTESIAN_POINT('Ctrl Pts',(2.08167059018418,-1.,-0.580819952108064));
#25417=CARTESIAN_POINT('Ctrl Pts',(2.07715226767559,-1.,-0.576300797416845));
#25418=CARTESIAN_POINT('Ctrl Pts',(2.07261449292824,-1.,-0.571816823242603));
#25419=CARTESIAN_POINT('Ctrl Pts',(2.06805732997334,-1.,-0.567368421181087));
#25420=CARTESIAN_POINT('Ctrl Pts',(2.06348090160589,-1.,-0.562955993082262));
#25421=CARTESIAN_POINT('Ctrl Pts',(2.05888537756462,-1.,-0.558579940185152));
#25422=CARTESIAN_POINT('Ctrl Pts',(2.05427091604413,-1.,-0.554240657463906));
#25423=CARTESIAN_POINT('Ctrl Pts',(2.04963761077958,-1.,-0.549938525150295));
#25424=CARTESIAN_POINT('Ctrl Pts',(2.04498544714588,-1.,-0.54567390381743));
#25425=CARTESIAN_POINT('Ctrl Pts',(2.04031422690527,-1.,-0.541447120615659));
#25426=CARTESIAN_POINT('Ctrl Pts',(2.03562362954037,-1.,-0.537258489833262));
#25427=CARTESIAN_POINT('Ctrl Pts',(2.03091336214426,-1.,-0.533108355132977));
#25428=CARTESIAN_POINT('Ctrl Pts',(2.0261832908329,-1.,-0.528997127241914));
#25429=CARTESIAN_POINT('Ctrl Pts',(2.02143356304698,-1.,-0.524925318333476));
#25430=CARTESIAN_POINT('Ctrl Pts',(2.01666477917286,-1.,-0.520893590399371));
#25431=CARTESIAN_POINT('Ctrl Pts',(2.01187773939242,-1.,-0.516902681728687));
#25432=CARTESIAN_POINT('Ctrl Pts',(2.00707309946949,-1.,-0.512953306961793));
#25433=CARTESIAN_POINT('Ctrl Pts',(2.00225107134734,-1.,-0.509046069886157));
#25434=CARTESIAN_POINT('Ctrl Pts',(1.99741107463572,-1.,-0.505181361323026));
#25435=CARTESIAN_POINT('Ctrl Pts',(1.99255149126155,-1.,-0.501359287727146));
#25436=CARTESIAN_POINT('Ctrl Pts',(1.98767044752932,-1.,-0.497579909545574));
#25437=CARTESIAN_POINT('Ctrl Pts',(1.98276658761821,-1.,-0.493843476541495));
#25438=CARTESIAN_POINT('Ctrl Pts',(1.97783973019229,-1.,-0.490150627860953));
#25439=CARTESIAN_POINT('Ctrl Pts',(1.97289186263272,-1.,-0.486502692907659));
#25440=CARTESIAN_POINT('Ctrl Pts',(1.96792703422362,-1.,-0.482901662120691));
#25441=CARTESIAN_POINT('Ctrl Pts',(1.96294933055943,-1.,-0.479349583074855));
#25442=CARTESIAN_POINT('Ctrl Pts',(1.95796111148177,-1.,-0.475848034683176));
#25443=CARTESIAN_POINT('Ctrl Pts',(1.95296148278133,-1.,-0.472397672264072));
#25444=CARTESIAN_POINT('Ctrl Pts',(1.94794381136514,-1.,-0.468997482913135));
#25445=CARTESIAN_POINT('Ctrl Pts',(1.9428979419619,-1.,-0.46564546202603));
#25446=CARTESIAN_POINT('Ctrl Pts',(1.93781486640821,-1.,-0.462340031009057));
#25447=CARTESIAN_POINT('Ctrl Pts',(1.93269066517934,-1.,-0.459081234547926));
#25448=CARTESIAN_POINT('Ctrl Pts',(1.92753067150476,-1.,-0.455872005174371));
#25449=CARTESIAN_POINT('Ctrl Pts',(1.92235380648502,-1.,-0.452719478359433));
#25450=CARTESIAN_POINT('Ctrl Pts',(1.91718342555755,-1.,-0.449632260106662));
#25451=CARTESIAN_POINT('Ctrl Pts',(1.9120369998112,-1.,-0.446617343485711));
#25452=CARTESIAN_POINT('Ctrl Pts',(1.90691756144898,-1.,-0.443677556849151));
#25453=CARTESIAN_POINT('Ctrl Pts',(1.90180124389086,-1.,-0.440807833704038));
#25454=CARTESIAN_POINT('Ctrl Pts',(1.89663648956466,-1.,-0.437995003948244));
#25455=CARTESIAN_POINT('Ctrl Pts',(1.89136993975504,-1.,-0.435225660963383));
#25456=CARTESIAN_POINT('Ctrl Pts',(1.88596913666793,-1.,-0.432493038548748));
#25457=CARTESIAN_POINT('Ctrl Pts',(1.88044229001832,-1.,-0.429803062482345));
#25458=CARTESIAN_POINT('Ctrl Pts',(1.87486989291484,-1.,-0.427183828519102));
#25459=CARTESIAN_POINT('Ctrl Pts',(1.86937803944323,-1.,-0.424678177291359));
#25460=CARTESIAN_POINT('Ctrl Pts',(1.86408083334028,-1.,-0.422327307418275));
#25461=CARTESIAN_POINT('Ctrl Pts',(1.85903281096686,-1.,-0.42015728797562));
#25462=CARTESIAN_POINT('Ctrl Pts',(1.85417632856234,-1.,-0.418164129143534));
#25463=CARTESIAN_POINT('Ctrl Pts',(1.84929312929882,-1.,-0.416300022038864));
#25464=CARTESIAN_POINT('Ctrl Pts',(1.8440575707371,-1.,-0.41448743825434));
#25465=CARTESIAN_POINT('Ctrl Pts',(1.83808953475839,-1.,-0.412633125322162));
#25466=CARTESIAN_POINT('Ctrl Pts',(1.83100408895216,-1.,-0.410641256301675));
#25467=CARTESIAN_POINT('Ctrl Pts',(1.8224702267854,-1.,-0.408428948108534));
#25468=CARTESIAN_POINT('Ctrl Pts',(1.81223801813988,-1.,-0.405933518411838));
#25469=CARTESIAN_POINT('Ctrl Pts',(1.80012077176221,-1.,-0.403107976170441));
#25470=CARTESIAN_POINT('Ctrl Pts',(1.78598826347533,-1.,-0.399919403783081));
#25471=CARTESIAN_POINT('Ctrl Pts',(1.7697556004756,-1.,-0.39634619612042));
#25472=CARTESIAN_POINT('Ctrl Pts',(1.75137405313962,-1.,-0.392375812294307));
#25473=CARTESIAN_POINT('Ctrl Pts',(1.7349317097561,-1.,-0.388877023509192));
#25474=CARTESIAN_POINT('Ctrl Pts',(1.72162022246158,-1.,-0.38607079032701));
#25475=CARTESIAN_POINT('Ctrl Pts',(1.71231062891958,-1.,-0.384119047315542));
#25476=CARTESIAN_POINT('Ctrl Pts',(1.7075470150345,-1.,-0.383122945602004));
#25477=CARTESIAN_POINT('',(1.74236521665491,-1.,-0.163289472382896));
#25478=CARTESIAN_POINT('Origin',(0.,-1.,0.));
#25479=CARTESIAN_POINT('',(2.19890268624765,-1.,-0.0694764450219582));
#25480=CARTESIAN_POINT('Ctrl Pts',(1.74236521665491,-1.,-0.163289472382896));
#25481=CARTESIAN_POINT('Ctrl Pts',(1.7472034950333,-1.,-0.163814161002002));
#25482=CARTESIAN_POINT('Ctrl Pts',(1.75666056638427,-1.,-0.164834765707159));
#25483=CARTESIAN_POINT('Ctrl Pts',(1.77018771684844,-1.,-0.1662793551464));
#25484=CARTESIAN_POINT('Ctrl Pts',(1.7869064998507,-1.,-0.168032772805197));
#25485=CARTESIAN_POINT('Ctrl Pts',(1.80561530629706,-1.,-0.169936923904608));
#25486=CARTESIAN_POINT('Ctrl Pts',(1.82215766811545,-1.,-0.171554770204119));
#25487=CARTESIAN_POINT('Ctrl Pts',(1.83658380527692,-1.,-0.1728894428919));
#25488=CARTESIAN_POINT('Ctrl Pts',(1.8489811319852,-1.,-0.173946627587732));
#25489=CARTESIAN_POINT('Ctrl Pts',(1.85948367088837,-1.,-0.17473525927603));
#25490=CARTESIAN_POINT('Ctrl Pts',(1.86828349694799,-1.,-0.175268337590758));
#25491=CARTESIAN_POINT('Ctrl Pts',(1.87563767773588,-1.,-0.175563480746485));
#25492=CARTESIAN_POINT('Ctrl Pts',(1.88188663145367,-1.,-0.175644148889699));
#25493=CARTESIAN_POINT('Ctrl Pts',(1.88742606273259,-1.,-0.175538155840648));
#25494=CARTESIAN_POINT('Ctrl Pts',(1.892646301985,-1.,-0.175274276190844));
#25495=CARTESIAN_POINT('Ctrl Pts',(1.89788101117132,-1.,-0.174879405091263));
#25496=CARTESIAN_POINT('Ctrl Pts',(1.90335253862834,-1.,-0.174375518661085));
#25497=CARTESIAN_POINT('Ctrl Pts',(1.90911693975267,-1.,-0.173776635257817));
#25498=CARTESIAN_POINT('Ctrl Pts',(1.91511429159527,-1.,-0.173090695383496));
#25499=CARTESIAN_POINT('Ctrl Pts',(1.9212233439798,-1.,-0.172321621259514));
#25500=CARTESIAN_POINT('Ctrl Pts',(1.92731093582036,-1.,-0.171471191532988));
#25501=CARTESIAN_POINT('Ctrl Pts',(1.93329183155539,-1.,-0.170541253116202));
#25502=CARTESIAN_POINT('Ctrl Pts',(1.93915639211581,-1.,-0.169534904817491));
#25503=CARTESIAN_POINT('Ctrl Pts',(1.94493757756931,-1.,-0.168455741607556));
#25504=CARTESIAN_POINT('Ctrl Pts',(1.95069027794294,-1.,-0.167307501784476));
#25505=CARTESIAN_POINT('Ctrl Pts',(1.9564675971873,-1.,-0.166093592002813));
#25506=CARTESIAN_POINT('Ctrl Pts',(1.96229379940136,-1.,-0.164816568920269));
#25507=CARTESIAN_POINT('Ctrl Pts',(1.96816512677967,-1.,-0.163478185457734));
#25508=CARTESIAN_POINT('Ctrl Pts',(1.97406280235188,-1.,-0.162079693556289));
#25509=CARTESIAN_POINT('Ctrl Pts',(1.97996195437559,-1.,-0.160622060784611));
#25510=CARTESIAN_POINT('Ctrl Pts',(1.98584238283292,-1.,-0.159106226437299));
#25511=CARTESIAN_POINT('Ctrl Pts',(1.99169810931908,-1.,-0.157533331459227));
#25512=CARTESIAN_POINT('Ctrl Pts',(1.99753284771497,-1.,-0.155904629548784));
#25513=CARTESIAN_POINT('Ctrl Pts',(2.00335565310543,-1.,-0.154221403049722));
#25514=CARTESIAN_POINT('Ctrl Pts',(2.00917680318424,-1.,-0.15248488362145));
#25515=CARTESIAN_POINT('Ctrl Pts',(2.01500291940238,-1.,-0.150696157673078));
#25516=CARTESIAN_POINT('Ctrl Pts',(2.02083464969894,-1.,-0.148856124775337));
#25517=CARTESIAN_POINT('Ctrl Pts',(2.02666926182017,-1.,-0.146965557332583));
#25518=CARTESIAN_POINT('Ctrl Pts',(2.03250223739942,-1.,-0.145025140186058));
#25519=CARTESIAN_POINT('Ctrl Pts',(2.03832911025912,-1.,-0.143035515058209));
#25520=CARTESIAN_POINT('Ctrl Pts',(2.04414757947916,-1.,-0.140997332152546));
#25521=CARTESIAN_POINT('Ctrl Pts',(2.04995762001328,-1.,-0.138911255368966));
#25522=CARTESIAN_POINT('Ctrl Pts',(2.05576044414264,-1.,-0.136777941218044));
#25523=CARTESIAN_POINT('Ctrl Pts',(2.06155781517842,-1.,-0.134598026192106));
#25524=CARTESIAN_POINT('Ctrl Pts',(2.06735123910326,-1.,-0.132372111547711));
#25525=CARTESIAN_POINT('Ctrl Pts',(2.07314114713063,-1.,-0.130100748328404));
#25526=CARTESIAN_POINT('Ctrl Pts',(2.07892715110987,-1.,-0.12778444527612));
#25527=CARTESIAN_POINT('Ctrl Pts',(2.08470840653643,-1.,-0.125423679412062));
#25528=CARTESIAN_POINT('Ctrl Pts',(2.09048392424825,-1.,-0.123018905621083));
#25529=CARTESIAN_POINT('Ctrl Pts',(2.0962529286773,-1.,-0.120570567965122));
#25530=CARTESIAN_POINT('Ctrl Pts',(2.102015121329,-1.,-0.118079107988356));
#25531=CARTESIAN_POINT('Ctrl Pts',(2.10777050261309,-1.,-0.115544957687927));
#25532=CARTESIAN_POINT('Ctrl Pts',(2.11351924490306,-1.,-0.112968534419737));
#25533=CARTESIAN_POINT('Ctrl Pts',(2.11926155590865,-1.,-0.110350236135025));
#25534=CARTESIAN_POINT('Ctrl Pts',(2.12499752307,-1.,-0.10769043523109));
#25535=CARTESIAN_POINT('Ctrl Pts',(2.13072704887293,-1.,-0.10498947915274));
#25536=CARTESIAN_POINT('Ctrl Pts',(2.13644992667165,-1.,-0.102247700556101));
#25537=CARTESIAN_POINT('Ctrl Pts',(2.14216588396025,-1.,-0.0994654261990917));
#25538=CARTESIAN_POINT('Ctrl Pts',(2.14787463531795,-1.,-0.096642985230546));
#25539=CARTESIAN_POINT('Ctrl Pts',(2.1535759397817,-1.,-0.0937807218867645));
#25540=CARTESIAN_POINT('Ctrl Pts',(2.15926961544516,-1.,-0.0908789888107267));
#25541=CARTESIAN_POINT('Ctrl Pts',(2.16495552645014,-1.,-0.0879381291386924));
#25542=CARTESIAN_POINT('Ctrl Pts',(2.17063357870952,-1.,-0.0849584620835374));
#25543=CARTESIAN_POINT('Ctrl Pts',(2.176303712113,-1.,-0.0819402680872767));
#25544=CARTESIAN_POINT('Ctrl Pts',(2.18196589448887,-1.,-0.0788837727685244));
#25545=CARTESIAN_POINT('Ctrl Pts',(2.1876201139953,-1.,-0.0757891465836149));
#25546=CARTESIAN_POINT('Ctrl Pts',(2.19213712013662,-1.,-0.0732830357306726));
#25547=CARTESIAN_POINT('Ctrl Pts',(2.19552129484002,-1.,-0.0713863779526155));
#25548=CARTESIAN_POINT('Ctrl Pts',(2.19777582085423,-1.,-0.0701143536325491));
#25549=CARTESIAN_POINT('Ctrl Pts',(2.19890268624765,-1.,-0.0694764450219582));
#25550=CARTESIAN_POINT('',(2.19890268624765,-1.,0.0694764450219582));
#25551=CARTESIAN_POINT('',(2.19890268624765,-1.,-0.0694764450219582));
#25552=CARTESIAN_POINT('',(1.74236521665491,-1.,0.163289472382896));
#25553=CARTESIAN_POINT('Ctrl Pts',(2.19890268624765,-1.,0.0694764450219582));
#25554=CARTESIAN_POINT('Ctrl Pts',(2.19777582085261,-1.,0.0701143536324925));
#25555=CARTESIAN_POINT('Ctrl Pts',(2.19552129483562,-1.,0.0713863779524626));
#25556=CARTESIAN_POINT('Ctrl Pts',(2.19213712012956,-1.,0.0732830357304275));
#25557=CARTESIAN_POINT('Ctrl Pts',(2.1876201139874,-1.,0.075789146583341));
#25558=CARTESIAN_POINT('Ctrl Pts',(2.18196589448304,-1.,0.0788837727683226));
#25559=CARTESIAN_POINT('Ctrl Pts',(2.1763037121106,-1.,0.0819402680871938));
#25560=CARTESIAN_POINT('Ctrl Pts',(2.17063357871031,-1.,0.0849584620835642));
#25561=CARTESIAN_POINT('Ctrl Pts',(2.16495552645275,-1.,0.0879381291387821));
#25562=CARTESIAN_POINT('Ctrl Pts',(2.15926961544808,-1.,0.0908789888108265));
#25563=CARTESIAN_POINT('Ctrl Pts',(2.15357593978377,-1.,0.0937807218868344));
#25564=CARTESIAN_POINT('Ctrl Pts',(2.14787463531864,-1.,0.0966429852305688));
#25565=CARTESIAN_POINT('Ctrl Pts',(2.14216588395974,-1.,0.0994654261990741));
#25566=CARTESIAN_POINT('Ctrl Pts',(2.13644992667052,-1.,0.102247700556063));
#25567=CARTESIAN_POINT('Ctrl Pts',(2.1307270488718,-1.,0.104989479152703));
#25568=CARTESIAN_POINT('Ctrl Pts',(2.12499752306927,-1.,0.107690435231068));
#25569=CARTESIAN_POINT('Ctrl Pts',(2.11926155590849,-1.,0.11035023613502));
#25570=CARTESIAN_POINT('Ctrl Pts',(2.11351924490335,-1.,0.112968534419746));
#25571=CARTESIAN_POINT('Ctrl Pts',(2.10777050261359,-1.,0.11554495768794));
#25572=CARTESIAN_POINT('Ctrl Pts',(2.10201512132945,-1.,0.118079107988368));
#25573=CARTESIAN_POINT('Ctrl Pts',(2.09625292867756,-1.,0.120570567965129));
#25574=CARTESIAN_POINT('Ctrl Pts',(2.09048392424826,-1.,0.123018905621083));
#25575=CARTESIAN_POINT('Ctrl Pts',(2.08470840653628,-1.,0.125423679412058));
#25576=CARTESIAN_POINT('Ctrl Pts',(2.07892715110967,-1.,0.127784445276116));
#25577=CARTESIAN_POINT('Ctrl Pts',(2.07314114713047,-1.,0.1301007483284));
#25578=CARTESIAN_POINT('Ctrl Pts',(2.06735123910319,-1.,0.132372111547709));
#25579=CARTESIAN_POINT('Ctrl Pts',(2.06155781517844,-1.,0.134598026192107));
#25580=CARTESIAN_POINT('Ctrl Pts',(2.0557604441427,-1.,0.136777941218044));
#25581=CARTESIAN_POINT('Ctrl Pts',(2.04995762001333,-1.,0.138911255368966));
#25582=CARTESIAN_POINT('Ctrl Pts',(2.04414757947919,-1.,0.140997332152545));
#25583=CARTESIAN_POINT('Ctrl Pts',(2.03832911025913,-1.,0.143035515058208));
#25584=CARTESIAN_POINT('Ctrl Pts',(2.03250223739941,-1.,0.145025140186058));
#25585=CARTESIAN_POINT('Ctrl Pts',(2.02666926182017,-1.,0.146965557332586));
#25586=CARTESIAN_POINT('Ctrl Pts',(2.02083464969897,-1.,0.148856124775342));
#25587=CARTESIAN_POINT('Ctrl Pts',(2.01500291940243,-1.,0.150696157673084));
#25588=CARTESIAN_POINT('Ctrl Pts',(2.00917680318426,-1.,0.152484883621452));
#25589=CARTESIAN_POINT('Ctrl Pts',(2.00335565310539,-1.,0.154221403049719));
#25590=CARTESIAN_POINT('Ctrl Pts',(1.99753284771487,-1.,0.155904629548774));
#25591=CARTESIAN_POINT('Ctrl Pts',(1.99169810931893,-1.,0.157533331459215));
#25592=CARTESIAN_POINT('Ctrl Pts',(1.98584238283279,-1.,0.159106226437288));
#25593=CARTESIAN_POINT('Ctrl Pts',(1.97996195437557,-1.,0.16062206078461));
#25594=CARTESIAN_POINT('Ctrl Pts',(1.97406280235204,-1.,0.162079693556302));
#25595=CARTESIAN_POINT('Ctrl Pts',(1.96816512678,-1.,0.16347818545776));
#25596=CARTESIAN_POINT('Ctrl Pts',(1.96229379940174,-1.,0.1648165689203));
#25597=CARTESIAN_POINT('Ctrl Pts',(1.95646759718755,-1.,0.166093592002832));
#25598=CARTESIAN_POINT('Ctrl Pts',(1.95069027794286,-1.,0.167307501784469));
#25599=CARTESIAN_POINT('Ctrl Pts',(1.94493757756879,-1.,0.168455741607515));
#25600=CARTESIAN_POINT('Ctrl Pts',(1.93915639211497,-1.,0.169534904817425));
#25601=CARTESIAN_POINT('Ctrl Pts',(1.93329183155455,-1.,0.170541253116136));
#25602=CARTESIAN_POINT('Ctrl Pts',(1.92731093582,-1.,0.17147119153296));
#25603=CARTESIAN_POINT('Ctrl Pts',(1.92122334398034,-1.,0.172321621259556));
#25604=CARTESIAN_POINT('Ctrl Pts',(1.91511429159681,-1.,0.173090695383619));
#25605=CARTESIAN_POINT('Ctrl Pts',(1.90911693975475,-1.,0.173776635257983));
#25606=CARTESIAN_POINT('Ctrl Pts',(1.90335253863003,-1.,0.174375518661222));
#25607=CARTESIAN_POINT('Ctrl Pts',(1.89788101117148,-1.,0.174879405091277));
#25608=CARTESIAN_POINT('Ctrl Pts',(1.89264630198279,-1.,0.175274276190664));
#25609=CARTESIAN_POINT('Ctrl Pts',(1.88742606272818,-1.,0.175538155840286));
#25610=CARTESIAN_POINT('Ctrl Pts',(1.88188663144846,-1.,0.175644148889271));
#25611=CARTESIAN_POINT('Ctrl Pts',(1.87563767773249,-1.,0.175563480746205));
#25612=CARTESIAN_POINT('Ctrl Pts',(1.86828349694972,-1.,0.1752683375909));
#25613=CARTESIAN_POINT('Ctrl Pts',(1.85948367089838,-1.,0.174735259276856));
#25614=CARTESIAN_POINT('Ctrl Pts',(1.84898113200543,-1.,0.173946627589401));
#25615=CARTESIAN_POINT('Ctrl Pts',(1.83658380530747,-1.,0.17288944289442));
#25616=CARTESIAN_POINT('Ctrl Pts',(1.82215766815414,-1.,0.171554770207306));
#25617=CARTESIAN_POINT('Ctrl Pts',(1.80561530633924,-1.,0.169936923908078));
#25618=CARTESIAN_POINT('Ctrl Pts',(1.78690649988931,-1.,0.16803277280837));
#25619=CARTESIAN_POINT('Ctrl Pts',(1.77018771687692,-1.,0.166279355148738));
#25620=CARTESIAN_POINT('Ctrl Pts',(1.75666056640041,-1.,0.164834765708484));
#25621=CARTESIAN_POINT('Ctrl Pts',(1.74720349503904,-1.,0.163814161002474));
#25622=CARTESIAN_POINT('Ctrl Pts',(1.74236521665491,-1.,0.163289472382896));
#25623=CARTESIAN_POINT('',(1.7075470150345,-1.,0.383122945602004));
#25624=CARTESIAN_POINT('Origin',(0.,-1.,0.));
#25625=CARTESIAN_POINT('',(2.11275013067528,-1.,0.613422273260091));
#25626=CARTESIAN_POINT('Ctrl Pts',(1.7075470150345,-1.,0.383122945602004));
#25627=CARTESIAN_POINT('Ctrl Pts',(1.71231062891398,-1.,0.384119047314215));
#25628=CARTESIAN_POINT('Ctrl Pts',(1.72162022244582,-1.,0.386070790323281));
#25629=CARTESIAN_POINT('Ctrl Pts',(1.73493170972829,-1.,0.388877023502615));
#25630=CARTESIAN_POINT('Ctrl Pts',(1.75137405310193,-1.,0.392375812285396));
#25631=CARTESIAN_POINT('Ctrl Pts',(1.76975560043442,-1.,0.396346196110688));
#25632=CARTESIAN_POINT('Ctrl Pts',(1.78598826343754,-1.,0.399919403774156));
#25633=CARTESIAN_POINT('Ctrl Pts',(1.80012077173238,-1.,0.403107976163396));
#25634=CARTESIAN_POINT('Ctrl Pts',(1.81223801812013,-1.,0.405933518407176));
#25635=CARTESIAN_POINT('Ctrl Pts',(1.82247022677562,-1.,0.408428948106228));
#25636=CARTESIAN_POINT('Ctrl Pts',(1.83100408895047,-1.,0.410641256301276));
#25637=CARTESIAN_POINT('Ctrl Pts',(1.8380895347617,-1.,0.412633125322945));
#25638=CARTESIAN_POINT('Ctrl Pts',(1.84405757074218,-1.,0.414487438255542));
#25639=CARTESIAN_POINT('Ctrl Pts',(1.84929312930314,-1.,0.416300022039885));
#25640=CARTESIAN_POINT('Ctrl Pts',(1.8541763285645,-1.,0.418164129144046));
#25641=CARTESIAN_POINT('Ctrl Pts',(1.8590328109667,-1.,0.420157287975583));
#25642=CARTESIAN_POINT('Ctrl Pts',(1.86408083333863,-1.,0.422327307417885));
#25643=CARTESIAN_POINT('Ctrl Pts',(1.8693780394412,-1.,0.424678177290876));
#25644=CARTESIAN_POINT('Ctrl Pts',(1.87486989291333,-1.,0.427183828518743));
#25645=CARTESIAN_POINT('Ctrl Pts',(1.88044229001778,-1.,0.429803062482217));
#25646=CARTESIAN_POINT('Ctrl Pts',(1.88596913666828,-1.,0.432493038548833));
#25647=CARTESIAN_POINT('Ctrl Pts',(1.89136993975585,-1.,0.43522566096358));
#25648=CARTESIAN_POINT('Ctrl Pts',(1.89663648956549,-1.,0.437995003948443));
#25649=CARTESIAN_POINT('Ctrl Pts',(1.90180124389137,-1.,0.440807833704161));
#25650=CARTESIAN_POINT('Ctrl Pts',(1.90691756144906,-1.,0.443677556849171));
#25651=CARTESIAN_POINT('Ctrl Pts',(1.91203699981095,-1.,0.446617343485651));
#25652=CARTESIAN_POINT('Ctrl Pts',(1.91718342555717,-1.,0.449632260106572));
#25653=CARTESIAN_POINT('Ctrl Pts',(1.9223538064847,-1.,0.452719478359356));
#25654=CARTESIAN_POINT('Ctrl Pts',(1.92753067150461,-1.,0.455872005174336));
#25655=CARTESIAN_POINT('Ctrl Pts',(1.93269066517936,-1.,0.459081234547932));
#25656=CARTESIAN_POINT('Ctrl Pts',(1.93781486640834,-1.,0.462340031009087));
#25657=CARTESIAN_POINT('Ctrl Pts',(1.94289794196205,-1.,0.465645462026065));
#25658=CARTESIAN_POINT('Ctrl Pts',(1.94794381136524,-1.,0.468997482913158));
#25659=CARTESIAN_POINT('Ctrl Pts',(1.95296148278136,-1.,0.47239767226408));
#25660=CARTESIAN_POINT('Ctrl Pts',(1.95796111148175,-1.,0.475848034683172));
#25661=CARTESIAN_POINT('Ctrl Pts',(1.96294933055938,-1.,0.479349583074846));
#25662=CARTESIAN_POINT('Ctrl Pts',(1.96792703422358,-1.,0.482901662120687));
#25663=CARTESIAN_POINT('Ctrl Pts',(1.97289186263272,-1.,0.486502692907661));
#25664=CARTESIAN_POINT('Ctrl Pts',(1.97783973019229,-1.,0.490150627860955));
#25665=CARTESIAN_POINT('Ctrl Pts',(1.9827665876182,-1.,0.493843476541493));
#25666=CARTESIAN_POINT('Ctrl Pts',(1.98767044752929,-1.,0.497579909545564));
#25667=CARTESIAN_POINT('Ctrl Pts',(1.9925514912615,-1.,0.501359287727129));
#25668=CARTESIAN_POINT('Ctrl Pts',(1.99741107463567,-1.,0.505181361323011));
#25669=CARTESIAN_POINT('Ctrl Pts',(2.00225107134733,-1.,0.509046069886152));
#25670=CARTESIAN_POINT('Ctrl Pts',(2.00707309946955,-1.,0.512953306961814));
#25671=CARTESIAN_POINT('Ctrl Pts',(2.01187773939257,-1.,0.516902681728733));
#25672=CARTESIAN_POINT('Ctrl Pts',(2.01666477917305,-1.,0.520893590399429));
#25673=CARTESIAN_POINT('Ctrl Pts',(2.02143356304712,-1.,0.524925318333519));
#25674=CARTESIAN_POINT('Ctrl Pts',(2.02618329083289,-1.,0.528997127241911));
#25675=CARTESIAN_POINT('Ctrl Pts',(2.03091336214401,-1.,0.533108355132905));
#25676=CARTESIAN_POINT('Ctrl Pts',(2.03562362953993,-1.,0.537258489833135));
#25677=CARTESIAN_POINT('Ctrl Pts',(2.0403142269048,-1.,0.54144712061552));
#25678=CARTESIAN_POINT('Ctrl Pts',(2.0449854471456,-1.,0.545673903817349));
#25679=CARTESIAN_POINT('Ctrl Pts',(2.04963761077974,-1.,0.549938525150342));
#25680=CARTESIAN_POINT('Ctrl Pts',(2.05427091604482,-1.,0.55424065746411));
#25681=CARTESIAN_POINT('Ctrl Pts',(2.05888537756571,-1.,0.558579940185468));
#25682=CARTESIAN_POINT('Ctrl Pts',(2.06348090160697,-1.,0.562955993082574));
#25683=CARTESIAN_POINT('Ctrl Pts',(2.06805732997383,-1.,0.56736842118123));
#25684=CARTESIAN_POINT('Ctrl Pts',(2.07261449292757,-1.,0.571816823242411));
#25685=CARTESIAN_POINT('Ctrl Pts',(2.07715226767361,-1.,0.576300797416275));
#25686=CARTESIAN_POINT('Ctrl Pts',(2.08167059018138,-1.,0.580819952107257));
#25687=CARTESIAN_POINT('Ctrl Pts',(2.086169437277,-1.,0.585373918990895));
#25688=CARTESIAN_POINT('Ctrl Pts',(2.09064881812053,-1.,0.58996236540319));
#25689=CARTESIAN_POINT('Ctrl Pts',(2.09510876220501,-1.,0.594585006052824));
#25690=CARTESIAN_POINT('Ctrl Pts',(2.09954930865331,-1.,0.599241616422144));
#25691=CARTESIAN_POINT('Ctrl Pts',(2.10397049887709,-1.,0.603932030738212));
#25692=CARTESIAN_POINT('Ctrl Pts',(2.10749199615859,-1.,0.607711315456826));
#25693=CARTESIAN_POINT('Ctrl Pts',(2.11012443807661,-1.,0.610560911691114));
#25694=CARTESIAN_POINT('Ctrl Pts',(2.11187554260142,-1.,0.61246736556225));
#25695=CARTESIAN_POINT('Ctrl Pts',(2.11275013067528,-1.,0.613422273260091));
#25696=CARTESIAN_POINT('',(2.0698113262342,-1.,0.745574324794401));
#25697=CARTESIAN_POINT('',(2.11275013067528,-1.,0.613422273260091));
#25698=CARTESIAN_POINT('Ctrl Pts',(2.0698113262342,-1.,0.745574324794401));
#25699=CARTESIAN_POINT('Ctrl Pts',(2.06854248895575,-1.,0.74583279137781));
#25700=CARTESIAN_POINT('Ctrl Pts',(2.06600523016401,-1.,0.746345871542696));
#25701=CARTESIAN_POINT('Ctrl Pts',(2.06220058927162,-1.,0.747103932785504));
#25702=CARTESIAN_POINT('Ctrl Pts',(2.05713023030263,-1.,0.748091554181101));
#25703=CARTESIAN_POINT('Ctrl Pts',(2.05079645591606,-1.,0.749287468663053));
#25704=CARTESIAN_POINT('Ctrl Pts',(2.04446689147754,-1.,0.750444657874758));
#25705=CARTESIAN_POINT('Ctrl Pts',(2.03814160092173,-1.,0.751562963361384));
#25706=CARTESIAN_POINT('Ctrl Pts',(2.03182068456467,-1.,0.752642180488104));
#25707=CARTESIAN_POINT('Ctrl Pts',(2.02550428623587,-1.,0.753682061113766));
#25708=CARTESIAN_POINT('Ctrl Pts',(2.01919259406003,-1.,0.75468233072352));
#25709=CARTESIAN_POINT('Ctrl Pts',(2.01288584328149,-1.,0.755642704958101));
#25710=CARTESIAN_POINT('Ctrl Pts',(2.00658431587682,-1.,0.756562904646496));
#25711=CARTESIAN_POINT('Ctrl Pts',(2.00028834739072,-1.,0.757442676862342));
#25712=CARTESIAN_POINT('Ctrl Pts',(1.9939983109871,-1.,0.758281796766377));
#25713=CARTESIAN_POINT('Ctrl Pts',(1.98771456680806,-1.,0.759080037802243));
#25714=CARTESIAN_POINT('Ctrl Pts',(1.98143741418156,-1.,0.759837147452135));
#25715=CARTESIAN_POINT('Ctrl Pts',(1.97516705321521,-1.,0.760552825409856));
#25716=CARTESIAN_POINT('Ctrl Pts',(1.96890351582545,-1.,0.761226690483986));
#25717=CARTESIAN_POINT('Ctrl Pts',(1.96264672744229,-1.,0.761858300014575));
#25718=CARTESIAN_POINT('Ctrl Pts',(1.95639665309893,-1.,0.762447203806264));
#25719=CARTESIAN_POINT('Ctrl Pts',(1.95015342590025,-1.,0.762992990878774));
#25720=CARTESIAN_POINT('Ctrl Pts',(1.94391746617626,-1.,0.763495333538581));
#25721=CARTESIAN_POINT('Ctrl Pts',(1.93768964875867,-1.,0.763954049121394));
#25722=CARTESIAN_POINT('Ctrl Pts',(1.93147105496367,-1.,0.76436901067389));
#25723=CARTESIAN_POINT('Ctrl Pts',(1.92526263537041,-1.,0.764740025488189));
#25724=CARTESIAN_POINT('Ctrl Pts',(1.91906491634197,-1.,0.765066729667095));
#25725=CARTESIAN_POINT('Ctrl Pts',(1.91287765805174,-1.,0.765348465884739));
#25726=CARTESIAN_POINT('Ctrl Pts',(1.90669961402362,-1.,0.765584196937937));
#25727=CARTESIAN_POINT('Ctrl Pts',(1.90052930393599,-1.,0.765772772593395));
#25728=CARTESIAN_POINT('Ctrl Pts',(1.89436577771389,-1.,0.765913193856979));
#25729=CARTESIAN_POINT('Ctrl Pts',(1.88820926433409,-1.,0.76600483706209));
#25730=CARTESIAN_POINT('Ctrl Pts',(1.88206215302561,-1.,0.766047794851869));
#25731=CARTESIAN_POINT('Ctrl Pts',(1.87592888967886,-1.,0.766042837036759));
#25732=CARTESIAN_POINT('Ctrl Pts',(1.86981398314345,-1.,0.765990708546112));
#25733=CARTESIAN_POINT('Ctrl Pts',(1.86372027063314,-1.,0.765891519092557));
#25734=CARTESIAN_POINT('Ctrl Pts',(1.85764741390391,-1.,0.765744212909305));
#25735=CARTESIAN_POINT('Ctrl Pts',(1.85158945130054,-1.,0.765545710619023));
#25736=CARTESIAN_POINT('Ctrl Pts',(1.8455369887591,-1.,0.765291664861972));
#25737=CARTESIAN_POINT('Ctrl Pts',(1.83948181064823,-1.,0.764978057881688));
#25738=CARTESIAN_POINT('Ctrl Pts',(1.8334207722714,-1.,0.764602549687846));
#25739=CARTESIAN_POINT('Ctrl Pts',(1.8273599120008,-1.,0.764165902606056));
#25740=CARTESIAN_POINT('Ctrl Pts',(1.82131873145297,-1.,0.763673465462854));
#25741=CARTESIAN_POINT('Ctrl Pts',(1.81532118405566,-1.,0.763132003836783));
#25742=CARTESIAN_POINT('Ctrl Pts',(1.80938551463989,-1.,0.762546129464036));
#25743=CARTESIAN_POINT('Ctrl Pts',(1.80351583877334,-1.,0.761915336443516));
#25744=CARTESIAN_POINT('Ctrl Pts',(1.79768986997735,-1.,0.761229695230359));
#25745=CARTESIAN_POINT('Ctrl Pts',(1.79185815610802,-1.,0.760469555880425));
#25746=CARTESIAN_POINT('Ctrl Pts',(1.78596964884526,-1.,0.759614401109868));
#25747=CARTESIAN_POINT('Ctrl Pts',(1.77999411220912,-1.,0.75865062667738));
#25748=CARTESIAN_POINT('Ctrl Pts',(1.77394167108342,-1.,0.757578264077238));
#25749=CARTESIAN_POINT('Ctrl Pts',(1.76789396003141,-1.,0.756421896028403));
#25750=CARTESIAN_POINT('Ctrl Pts',(1.7619781724032,-1.,0.755220979975262));
#25751=CARTESIAN_POINT('Ctrl Pts',(1.75631083600175,-1.,0.75400925402848));
#25752=CARTESIAN_POINT('Ctrl Pts',(1.75095139468809,-1.,0.752797683531377));
#25753=CARTESIAN_POINT('Ctrl Pts',(1.74585086852298,-1.,0.751555614163629));
#25754=CARTESIAN_POINT('Ctrl Pts',(1.74080458266705,-1.,0.750193435979541));
#25755=CARTESIAN_POINT('Ctrl Pts',(1.73550351679848,-1.,0.748582462954855));
#25756=CARTESIAN_POINT('Ctrl Pts',(1.72958533647399,-1.,0.746574710096437));
#25757=CARTESIAN_POINT('Ctrl Pts',(1.7226822991693,-1.,0.744021445433765));
#25758=CARTESIAN_POINT('Ctrl Pts',(1.71447789751927,-1.,0.740795162032088));
#25759=CARTESIAN_POINT('Ctrl Pts',(1.70473309006121,-1.,0.736799665724771));
#25760=CARTESIAN_POINT('Ctrl Pts',(1.69326921975743,-1.,0.731963238697195));
#25761=CARTESIAN_POINT('Ctrl Pts',(1.67996158455503,-1.,0.726235967997433));
#25762=CARTESIAN_POINT('Ctrl Pts',(1.6647288055568,-1.,0.719585433804282));
#25763=CARTESIAN_POINT('Ctrl Pts',(1.64752408832016,-1.,0.711993139355394));
#25764=CARTESIAN_POINT('Ctrl Pts',(1.63216541664676,-1.,0.705159151988319));
#25765=CARTESIAN_POINT('Ctrl Pts',(1.61974673472612,-1.,0.699605146405088));
#25766=CARTESIAN_POINT('Ctrl Pts',(1.61106790958151,-1.,0.695712097881194));
#25767=CARTESIAN_POINT('Ctrl Pts',(1.60662857109684,-1.,0.693717979106306));
#25768=CARTESIAN_POINT('Origin',(0.,-1.,0.));
#25769=CARTESIAN_POINT('Origin',(0.,0.,0.));
#25770=CARTESIAN_POINT('Origin',(0.,2.2,0.));
#25771=CARTESIAN_POINT('Origin',(0.,1.,0.));
#25772=CARTESIAN_POINT('',(-1.4,2.2,1.71450551880629E-16));
#25773=CARTESIAN_POINT('Origin',(0.,2.2,0.));
#25774=CARTESIAN_POINT('',(-1.4,1.,1.71450551880629E-16));
#25775=CARTESIAN_POINT('',(-1.4,1.,1.71450551880629E-16));
#25776=CARTESIAN_POINT('Origin',(0.,1.,0.));
#25777=CARTESIAN_POINT('Origin',(0.,2.2,0.));
#25778=CARTESIAN_POINT('Ctrl Pts',(2.11275013067528,-1.,0.613422273260091));
#25779=CARTESIAN_POINT('Ctrl Pts',(2.11275013067528,1.,0.613422273260091));
#25780=CARTESIAN_POINT('Ctrl Pts',(2.11187554260142,-1.,0.61246736556225));
#25781=CARTESIAN_POINT('Ctrl Pts',(2.11187554260142,1.,0.61246736556225));
#25782=CARTESIAN_POINT('Ctrl Pts',(2.11012443807661,-1.,0.610560911691114));
#25783=CARTESIAN_POINT('Ctrl Pts',(2.11012443807661,1.,0.610560911691114));
#25784=CARTESIAN_POINT('Ctrl Pts',(2.10749199615859,-1.,0.607711315456826));
#25785=CARTESIAN_POINT('Ctrl Pts',(2.10749199615859,1.,0.607711315456826));
#25786=CARTESIAN_POINT('Ctrl Pts',(2.10397049887709,-1.,0.603932030738212));
#25787=CARTESIAN_POINT('Ctrl Pts',(2.10397049887709,1.,0.603932030738212));
#25788=CARTESIAN_POINT('Ctrl Pts',(2.09954930865331,-1.,0.599241616422144));
#25789=CARTESIAN_POINT('Ctrl Pts',(2.09954930865331,1.,0.599241616422144));
#25790=CARTESIAN_POINT('Ctrl Pts',(2.09510876220501,-1.,0.594585006052824));
#25791=CARTESIAN_POINT('Ctrl Pts',(2.09510876220501,1.,0.594585006052824));
#25792=CARTESIAN_POINT('Ctrl Pts',(2.09064881812053,-1.,0.58996236540319));
#25793=CARTESIAN_POINT('Ctrl Pts',(2.09064881812053,1.,0.58996236540319));
#25794=CARTESIAN_POINT('Ctrl Pts',(2.086169437277,-1.,0.585373918990895));
#25795=CARTESIAN_POINT('Ctrl Pts',(2.086169437277,1.,0.585373918990895));
#25796=CARTESIAN_POINT('Ctrl Pts',(2.08167059018138,-1.,0.580819952107257));
#25797=CARTESIAN_POINT('Ctrl Pts',(2.08167059018138,1.,0.580819952107257));
#25798=CARTESIAN_POINT('Ctrl Pts',(2.07715226767361,-1.,0.576300797416275));
#25799=CARTESIAN_POINT('Ctrl Pts',(2.07715226767361,1.,0.576300797416275));
#25800=CARTESIAN_POINT('Ctrl Pts',(2.07261449292757,-1.,0.571816823242411));
#25801=CARTESIAN_POINT('Ctrl Pts',(2.07261449292757,1.,0.571816823242411));
#25802=CARTESIAN_POINT('Ctrl Pts',(2.06805732997383,-1.,0.56736842118123));
#25803=CARTESIAN_POINT('Ctrl Pts',(2.06805732997383,1.,0.56736842118123));
#25804=CARTESIAN_POINT('Ctrl Pts',(2.06348090160697,-1.,0.562955993082574));
#25805=CARTESIAN_POINT('Ctrl Pts',(2.06348090160697,1.,0.562955993082574));
#25806=CARTESIAN_POINT('Ctrl Pts',(2.05888537756571,-1.,0.558579940185468));
#25807=CARTESIAN_POINT('Ctrl Pts',(2.05888537756571,1.,0.558579940185468));
#25808=CARTESIAN_POINT('Ctrl Pts',(2.05427091604482,-1.,0.55424065746411));
#25809=CARTESIAN_POINT('Ctrl Pts',(2.05427091604482,1.,0.55424065746411));
#25810=CARTESIAN_POINT('Ctrl Pts',(2.04963761077974,-1.,0.549938525150342));
#25811=CARTESIAN_POINT('Ctrl Pts',(2.04963761077974,1.,0.549938525150342));
#25812=CARTESIAN_POINT('Ctrl Pts',(2.0449854471456,-1.,0.545673903817349));
#25813=CARTESIAN_POINT('Ctrl Pts',(2.0449854471456,1.,0.545673903817349));
#25814=CARTESIAN_POINT('Ctrl Pts',(2.0403142269048,-1.,0.54144712061552));
#25815=CARTESIAN_POINT('Ctrl Pts',(2.0403142269048,1.,0.54144712061552));
#25816=CARTESIAN_POINT('Ctrl Pts',(2.03562362953993,-1.,0.537258489833135));
#25817=CARTESIAN_POINT('Ctrl Pts',(2.03562362953993,1.,0.537258489833135));
#25818=CARTESIAN_POINT('Ctrl Pts',(2.03091336214401,-1.,0.533108355132905));
#25819=CARTESIAN_POINT('Ctrl Pts',(2.03091336214401,1.,0.533108355132905));
#25820=CARTESIAN_POINT('Ctrl Pts',(2.02618329083289,-1.,0.528997127241911));
#25821=CARTESIAN_POINT('Ctrl Pts',(2.02618329083289,1.,0.528997127241911));
#25822=CARTESIAN_POINT('Ctrl Pts',(2.02143356304712,-1.,0.524925318333519));
#25823=CARTESIAN_POINT('Ctrl Pts',(2.02143356304712,1.,0.524925318333519));
#25824=CARTESIAN_POINT('Ctrl Pts',(2.01666477917305,-1.,0.520893590399429));
#25825=CARTESIAN_POINT('Ctrl Pts',(2.01666477917305,1.,0.520893590399429));
#25826=CARTESIAN_POINT('Ctrl Pts',(2.01187773939257,-1.,0.516902681728733));
#25827=CARTESIAN_POINT('Ctrl Pts',(2.01187773939257,1.,0.516902681728733));
#25828=CARTESIAN_POINT('Ctrl Pts',(2.00707309946955,-1.,0.512953306961814));
#25829=CARTESIAN_POINT('Ctrl Pts',(2.00707309946955,1.,0.512953306961814));
#25830=CARTESIAN_POINT('Ctrl Pts',(2.00225107134733,-1.,0.509046069886152));
#25831=CARTESIAN_POINT('Ctrl Pts',(2.00225107134733,1.,0.509046069886152));
#25832=CARTESIAN_POINT('Ctrl Pts',(1.99741107463567,-1.,0.505181361323011));
#25833=CARTESIAN_POINT('Ctrl Pts',(1.99741107463567,1.,0.505181361323011));
#25834=CARTESIAN_POINT('Ctrl Pts',(1.9925514912615,-1.,0.501359287727129));
#25835=CARTESIAN_POINT('Ctrl Pts',(1.9925514912615,1.,0.501359287727129));
#25836=CARTESIAN_POINT('Ctrl Pts',(1.98767044752929,-1.,0.497579909545564));
#25837=CARTESIAN_POINT('Ctrl Pts',(1.98767044752929,1.,0.497579909545564));
#25838=CARTESIAN_POINT('Ctrl Pts',(1.9827665876182,-1.,0.493843476541493));
#25839=CARTESIAN_POINT('Ctrl Pts',(1.9827665876182,1.,0.493843476541493));
#25840=CARTESIAN_POINT('Ctrl Pts',(1.97783973019229,-1.,0.490150627860955));
#25841=CARTESIAN_POINT('Ctrl Pts',(1.97783973019229,1.,0.490150627860955));
#25842=CARTESIAN_POINT('Ctrl Pts',(1.97289186263272,-1.,0.486502692907661));
#25843=CARTESIAN_POINT('Ctrl Pts',(1.97289186263272,1.,0.486502692907661));
#25844=CARTESIAN_POINT('Ctrl Pts',(1.96792703422358,-1.,0.482901662120687));
#25845=CARTESIAN_POINT('Ctrl Pts',(1.96792703422358,1.,0.482901662120687));
#25846=CARTESIAN_POINT('Ctrl Pts',(1.96294933055938,-1.,0.479349583074846));
#25847=CARTESIAN_POINT('Ctrl Pts',(1.96294933055938,1.,0.479349583074846));
#25848=CARTESIAN_POINT('Ctrl Pts',(1.95796111148175,-1.,0.475848034683172));
#25849=CARTESIAN_POINT('Ctrl Pts',(1.95796111148175,1.,0.475848034683172));
#25850=CARTESIAN_POINT('Ctrl Pts',(1.95296148278136,-1.,0.47239767226408));
#25851=CARTESIAN_POINT('Ctrl Pts',(1.95296148278136,1.,0.47239767226408));
#25852=CARTESIAN_POINT('Ctrl Pts',(1.94794381136524,-1.,0.468997482913158));
#25853=CARTESIAN_POINT('Ctrl Pts',(1.94794381136524,1.,0.468997482913158));
#25854=CARTESIAN_POINT('Ctrl Pts',(1.94289794196205,-1.,0.465645462026065));
#25855=CARTESIAN_POINT('Ctrl Pts',(1.94289794196205,1.,0.465645462026065));
#25856=CARTESIAN_POINT('Ctrl Pts',(1.93781486640834,-1.,0.462340031009087));
#25857=CARTESIAN_POINT('Ctrl Pts',(1.93781486640834,1.,0.462340031009087));
#25858=CARTESIAN_POINT('Ctrl Pts',(1.93269066517936,-1.,0.459081234547932));
#25859=CARTESIAN_POINT('Ctrl Pts',(1.93269066517936,1.,0.459081234547932));
#25860=CARTESIAN_POINT('Ctrl Pts',(1.92753067150461,-1.,0.455872005174336));
#25861=CARTESIAN_POINT('Ctrl Pts',(1.92753067150461,1.,0.455872005174336));
#25862=CARTESIAN_POINT('Ctrl Pts',(1.9223538064847,-1.,0.452719478359356));
#25863=CARTESIAN_POINT('Ctrl Pts',(1.9223538064847,1.,0.452719478359356));
#25864=CARTESIAN_POINT('Ctrl Pts',(1.91718342555717,-1.,0.449632260106572));
#25865=CARTESIAN_POINT('Ctrl Pts',(1.91718342555717,1.,0.449632260106572));
#25866=CARTESIAN_POINT('Ctrl Pts',(1.91203699981095,-1.,0.446617343485651));
#25867=CARTESIAN_POINT('Ctrl Pts',(1.91203699981095,1.,0.446617343485651));
#25868=CARTESIAN_POINT('Ctrl Pts',(1.90691756144906,-1.,0.443677556849171));
#25869=CARTESIAN_POINT('Ctrl Pts',(1.90691756144906,1.,0.443677556849171));
#25870=CARTESIAN_POINT('Ctrl Pts',(1.90180124389137,-1.,0.440807833704161));
#25871=CARTESIAN_POINT('Ctrl Pts',(1.90180124389137,1.,0.440807833704161));
#25872=CARTESIAN_POINT('Ctrl Pts',(1.89663648956549,-1.,0.437995003948443));
#25873=CARTESIAN_POINT('Ctrl Pts',(1.89663648956549,1.,0.437995003948443));
#25874=CARTESIAN_POINT('Ctrl Pts',(1.89136993975585,-1.,0.43522566096358));
#25875=CARTESIAN_POINT('Ctrl Pts',(1.89136993975585,1.,0.43522566096358));
#25876=CARTESIAN_POINT('Ctrl Pts',(1.88596913666828,-1.,0.432493038548833));
#25877=CARTESIAN_POINT('Ctrl Pts',(1.88596913666828,1.,0.432493038548833));
#25878=CARTESIAN_POINT('Ctrl Pts',(1.88044229001778,-1.,0.429803062482217));
#25879=CARTESIAN_POINT('Ctrl Pts',(1.88044229001778,1.,0.429803062482217));
#25880=CARTESIAN_POINT('Ctrl Pts',(1.87486989291333,-1.,0.427183828518743));
#25881=CARTESIAN_POINT('Ctrl Pts',(1.87486989291333,1.,0.427183828518743));
#25882=CARTESIAN_POINT('Ctrl Pts',(1.8693780394412,-1.,0.424678177290876));
#25883=CARTESIAN_POINT('Ctrl Pts',(1.8693780394412,1.,0.424678177290876));
#25884=CARTESIAN_POINT('Ctrl Pts',(1.86408083333863,-1.,0.422327307417885));
#25885=CARTESIAN_POINT('Ctrl Pts',(1.86408083333863,1.,0.422327307417885));
#25886=CARTESIAN_POINT('Ctrl Pts',(1.8590328109667,-1.,0.420157287975583));
#25887=CARTESIAN_POINT('Ctrl Pts',(1.8590328109667,1.,0.420157287975583));
#25888=CARTESIAN_POINT('Ctrl Pts',(1.8541763285645,-1.,0.418164129144046));
#25889=CARTESIAN_POINT('Ctrl Pts',(1.8541763285645,1.,0.418164129144046));
#25890=CARTESIAN_POINT('Ctrl Pts',(1.84929312930314,-1.,0.416300022039885));
#25891=CARTESIAN_POINT('Ctrl Pts',(1.84929312930314,1.,0.416300022039885));
#25892=CARTESIAN_POINT('Ctrl Pts',(1.84405757074218,-1.,0.414487438255542));
#25893=CARTESIAN_POINT('Ctrl Pts',(1.84405757074218,1.,0.414487438255542));
#25894=CARTESIAN_POINT('Ctrl Pts',(1.8380895347617,-1.,0.412633125322945));
#25895=CARTESIAN_POINT('Ctrl Pts',(1.8380895347617,1.,0.412633125322945));
#25896=CARTESIAN_POINT('Ctrl Pts',(1.83100408895047,-1.,0.410641256301276));
#25897=CARTESIAN_POINT('Ctrl Pts',(1.83100408895047,1.,0.410641256301276));
#25898=CARTESIAN_POINT('Ctrl Pts',(1.82247022677562,-1.,0.408428948106228));
#25899=CARTESIAN_POINT('Ctrl Pts',(1.82247022677562,1.,0.408428948106228));
#25900=CARTESIAN_POINT('Ctrl Pts',(1.81223801812013,-1.,0.405933518407176));
#25901=CARTESIAN_POINT('Ctrl Pts',(1.81223801812013,1.,0.405933518407176));
#25902=CARTESIAN_POINT('Ctrl Pts',(1.80012077173238,-1.,0.403107976163396));
#25903=CARTESIAN_POINT('Ctrl Pts',(1.80012077173238,1.,0.403107976163396));
#25904=CARTESIAN_POINT('Ctrl Pts',(1.78598826343754,-1.,0.399919403774156));
#25905=CARTESIAN_POINT('Ctrl Pts',(1.78598826343754,1.,0.399919403774156));
#25906=CARTESIAN_POINT('Ctrl Pts',(1.76975560043442,-1.,0.396346196110688));
#25907=CARTESIAN_POINT('Ctrl Pts',(1.76975560043442,1.,0.396346196110688));
#25908=CARTESIAN_POINT('Ctrl Pts',(1.75137405310193,-1.,0.392375812285396));
#25909=CARTESIAN_POINT('Ctrl Pts',(1.75137405310193,1.,0.392375812285396));
#25910=CARTESIAN_POINT('Ctrl Pts',(1.73493170972829,-1.,0.388877023502615));
#25911=CARTESIAN_POINT('Ctrl Pts',(1.73493170972829,1.,0.388877023502615));
#25912=CARTESIAN_POINT('Ctrl Pts',(1.72162022244582,-1.,0.386070790323281));
#25913=CARTESIAN_POINT('Ctrl Pts',(1.72162022244582,1.,0.386070790323281));
#25914=CARTESIAN_POINT('Ctrl Pts',(1.71231062891398,-1.,0.384119047314215));
#25915=CARTESIAN_POINT('Ctrl Pts',(1.71231062891398,1.,0.384119047314215));
#25916=CARTESIAN_POINT('Ctrl Pts',(1.7075470150345,-1.,0.383122945602004));
#25917=CARTESIAN_POINT('Ctrl Pts',(1.7075470150345,1.,0.383122945602004));
#25918=CARTESIAN_POINT('',(1.7075470150345,1.,0.383122945602004));
#25919=CARTESIAN_POINT('',(1.7075470150345,0.,0.383122945602005));
#25920=CARTESIAN_POINT('',(2.11275013067528,1.,0.613422273260091));
#25921=CARTESIAN_POINT('Ctrl Pts',(2.11275013067528,1.,0.613422273260091));
#25922=CARTESIAN_POINT('Ctrl Pts',(2.11187554260142,1.,0.61246736556225));
#25923=CARTESIAN_POINT('Ctrl Pts',(2.11012443807661,1.,0.610560911691114));
#25924=CARTESIAN_POINT('Ctrl Pts',(2.10749199615859,1.,0.607711315456826));
#25925=CARTESIAN_POINT('Ctrl Pts',(2.10397049887709,1.,0.603932030738212));
#25926=CARTESIAN_POINT('Ctrl Pts',(2.09954930865331,1.,0.599241616422144));
#25927=CARTESIAN_POINT('Ctrl Pts',(2.09510876220501,1.,0.594585006052824));
#25928=CARTESIAN_POINT('Ctrl Pts',(2.09064881812053,1.,0.58996236540319));
#25929=CARTESIAN_POINT('Ctrl Pts',(2.086169437277,1.,0.585373918990895));
#25930=CARTESIAN_POINT('Ctrl Pts',(2.08167059018138,1.,0.580819952107257));
#25931=CARTESIAN_POINT('Ctrl Pts',(2.07715226767361,1.,0.576300797416275));
#25932=CARTESIAN_POINT('Ctrl Pts',(2.07261449292757,1.,0.571816823242411));
#25933=CARTESIAN_POINT('Ctrl Pts',(2.06805732997383,1.,0.56736842118123));
#25934=CARTESIAN_POINT('Ctrl Pts',(2.06348090160697,1.,0.562955993082574));
#25935=CARTESIAN_POINT('Ctrl Pts',(2.05888537756571,1.,0.558579940185468));
#25936=CARTESIAN_POINT('Ctrl Pts',(2.05427091604482,1.,0.55424065746411));
#25937=CARTESIAN_POINT('Ctrl Pts',(2.04963761077974,1.,0.549938525150342));
#25938=CARTESIAN_POINT('Ctrl Pts',(2.0449854471456,1.,0.545673903817349));
#25939=CARTESIAN_POINT('Ctrl Pts',(2.0403142269048,1.,0.54144712061552));
#25940=CARTESIAN_POINT('Ctrl Pts',(2.03562362953993,1.,0.537258489833135));
#25941=CARTESIAN_POINT('Ctrl Pts',(2.03091336214401,1.,0.533108355132905));
#25942=CARTESIAN_POINT('Ctrl Pts',(2.02618329083289,1.,0.528997127241911));
#25943=CARTESIAN_POINT('Ctrl Pts',(2.02143356304712,1.,0.524925318333519));
#25944=CARTESIAN_POINT('Ctrl Pts',(2.01666477917305,1.,0.520893590399429));
#25945=CARTESIAN_POINT('Ctrl Pts',(2.01187773939257,1.,0.516902681728733));
#25946=CARTESIAN_POINT('Ctrl Pts',(2.00707309946955,1.,0.512953306961814));
#25947=CARTESIAN_POINT('Ctrl Pts',(2.00225107134733,1.,0.509046069886152));
#25948=CARTESIAN_POINT('Ctrl Pts',(1.99741107463567,1.,0.505181361323011));
#25949=CARTESIAN_POINT('Ctrl Pts',(1.9925514912615,1.,0.501359287727129));
#25950=CARTESIAN_POINT('Ctrl Pts',(1.98767044752929,1.,0.497579909545564));
#25951=CARTESIAN_POINT('Ctrl Pts',(1.9827665876182,1.,0.493843476541493));
#25952=CARTESIAN_POINT('Ctrl Pts',(1.97783973019229,1.,0.490150627860955));
#25953=CARTESIAN_POINT('Ctrl Pts',(1.97289186263272,1.,0.486502692907661));
#25954=CARTESIAN_POINT('Ctrl Pts',(1.96792703422358,1.,0.482901662120687));
#25955=CARTESIAN_POINT('Ctrl Pts',(1.96294933055938,1.,0.479349583074846));
#25956=CARTESIAN_POINT('Ctrl Pts',(1.95796111148175,1.,0.475848034683172));
#25957=CARTESIAN_POINT('Ctrl Pts',(1.95296148278136,1.,0.47239767226408));
#25958=CARTESIAN_POINT('Ctrl Pts',(1.94794381136524,1.,0.468997482913158));
#25959=CARTESIAN_POINT('Ctrl Pts',(1.94289794196205,1.,0.465645462026065));
#25960=CARTESIAN_POINT('Ctrl Pts',(1.93781486640834,1.,0.462340031009087));
#25961=CARTESIAN_POINT('Ctrl Pts',(1.93269066517936,1.,0.459081234547932));
#25962=CARTESIAN_POINT('Ctrl Pts',(1.92753067150461,1.,0.455872005174336));
#25963=CARTESIAN_POINT('Ctrl Pts',(1.9223538064847,1.,0.452719478359356));
#25964=CARTESIAN_POINT('Ctrl Pts',(1.91718342555717,1.,0.449632260106572));
#25965=CARTESIAN_POINT('Ctrl Pts',(1.91203699981095,1.,0.446617343485651));
#25966=CARTESIAN_POINT('Ctrl Pts',(1.90691756144906,1.,0.443677556849171));
#25967=CARTESIAN_POINT('Ctrl Pts',(1.90180124389137,1.,0.440807833704161));
#25968=CARTESIAN_POINT('Ctrl Pts',(1.89663648956549,1.,0.437995003948443));
#25969=CARTESIAN_POINT('Ctrl Pts',(1.89136993975585,1.,0.43522566096358));
#25970=CARTESIAN_POINT('Ctrl Pts',(1.88596913666828,1.,0.432493038548833));
#25971=CARTESIAN_POINT('Ctrl Pts',(1.88044229001778,1.,0.429803062482217));
#25972=CARTESIAN_POINT('Ctrl Pts',(1.87486989291333,1.,0.427183828518743));
#25973=CARTESIAN_POINT('Ctrl Pts',(1.8693780394412,1.,0.424678177290876));
#25974=CARTESIAN_POINT('Ctrl Pts',(1.86408083333863,1.,0.422327307417885));
#25975=CARTESIAN_POINT('Ctrl Pts',(1.8590328109667,1.,0.420157287975583));
#25976=CARTESIAN_POINT('Ctrl Pts',(1.8541763285645,1.,0.418164129144046));
#25977=CARTESIAN_POINT('Ctrl Pts',(1.84929312930314,1.,0.416300022039885));
#25978=CARTESIAN_POINT('Ctrl Pts',(1.84405757074218,1.,0.414487438255542));
#25979=CARTESIAN_POINT('Ctrl Pts',(1.8380895347617,1.,0.412633125322945));
#25980=CARTESIAN_POINT('Ctrl Pts',(1.83100408895047,1.,0.410641256301276));
#25981=CARTESIAN_POINT('Ctrl Pts',(1.82247022677562,1.,0.408428948106228));
#25982=CARTESIAN_POINT('Ctrl Pts',(1.81223801812013,1.,0.405933518407176));
#25983=CARTESIAN_POINT('Ctrl Pts',(1.80012077173238,1.,0.403107976163396));
#25984=CARTESIAN_POINT('Ctrl Pts',(1.78598826343754,1.,0.399919403774156));
#25985=CARTESIAN_POINT('Ctrl Pts',(1.76975560043442,1.,0.396346196110688));
#25986=CARTESIAN_POINT('Ctrl Pts',(1.75137405310193,1.,0.392375812285396));
#25987=CARTESIAN_POINT('Ctrl Pts',(1.73493170972829,1.,0.388877023502615));
#25988=CARTESIAN_POINT('Ctrl Pts',(1.72162022244582,1.,0.386070790323281));
#25989=CARTESIAN_POINT('Ctrl Pts',(1.71231062891398,1.,0.384119047314215));
#25990=CARTESIAN_POINT('Ctrl Pts',(1.7075470150345,1.,0.383122945602004));
#25991=CARTESIAN_POINT('',(2.11275013067528,0.,0.613422273260091));
#25992=CARTESIAN_POINT('Origin',(2.0698113262342,0.,0.745574324794401));
#25993=CARTESIAN_POINT('',(2.0698113262342,1.,0.745574324794401));
#25994=CARTESIAN_POINT('',(2.11275013067528,1.,0.613422273260091));
#25995=CARTESIAN_POINT('',(2.0698113262342,0.,0.745574324794401));
#25996=CARTESIAN_POINT('Ctrl Pts',(1.60662857109684,-1.,0.693717979106306));
#25997=CARTESIAN_POINT('Ctrl Pts',(1.60662857109684,1.,0.693717979106306));
#25998=CARTESIAN_POINT('Ctrl Pts',(1.61106790958151,-1.,0.695712097881194));
#25999=CARTESIAN_POINT('Ctrl Pts',(1.61106790958151,1.,0.695712097881194));
#26000=CARTESIAN_POINT('Ctrl Pts',(1.61974673472612,-1.,0.699605146405088));
#26001=CARTESIAN_POINT('Ctrl Pts',(1.61974673472612,1.,0.699605146405088));
#26002=CARTESIAN_POINT('Ctrl Pts',(1.63216541664676,-1.,0.705159151988319));
#26003=CARTESIAN_POINT('Ctrl Pts',(1.63216541664676,1.,0.705159151988319));
#26004=CARTESIAN_POINT('Ctrl Pts',(1.64752408832016,-1.,0.711993139355394));
#26005=CARTESIAN_POINT('Ctrl Pts',(1.64752408832016,1.,0.711993139355394));
#26006=CARTESIAN_POINT('Ctrl Pts',(1.6647288055568,-1.,0.719585433804282));
#26007=CARTESIAN_POINT('Ctrl Pts',(1.6647288055568,1.,0.719585433804282));
#26008=CARTESIAN_POINT('Ctrl Pts',(1.67996158455503,-1.,0.726235967997433));
#26009=CARTESIAN_POINT('Ctrl Pts',(1.67996158455503,1.,0.726235967997433));
#26010=CARTESIAN_POINT('Ctrl Pts',(1.69326921975743,-1.,0.731963238697195));
#26011=CARTESIAN_POINT('Ctrl Pts',(1.69326921975743,1.,0.731963238697195));
#26012=CARTESIAN_POINT('Ctrl Pts',(1.70473309006121,-1.,0.736799665724771));
#26013=CARTESIAN_POINT('Ctrl Pts',(1.70473309006121,1.,0.736799665724771));
#26014=CARTESIAN_POINT('Ctrl Pts',(1.71447789751927,-1.,0.740795162032088));
#26015=CARTESIAN_POINT('Ctrl Pts',(1.71447789751927,1.,0.740795162032088));
#26016=CARTESIAN_POINT('Ctrl Pts',(1.7226822991693,-1.,0.744021445433765));
#26017=CARTESIAN_POINT('Ctrl Pts',(1.7226822991693,1.,0.744021445433765));
#26018=CARTESIAN_POINT('Ctrl Pts',(1.72958533647399,-1.,0.746574710096437));
#26019=CARTESIAN_POINT('Ctrl Pts',(1.72958533647399,1.,0.746574710096437));
#26020=CARTESIAN_POINT('Ctrl Pts',(1.73550351679848,-1.,0.748582462954855));
#26021=CARTESIAN_POINT('Ctrl Pts',(1.73550351679848,1.,0.748582462954855));
#26022=CARTESIAN_POINT('Ctrl Pts',(1.74080458266705,-1.,0.750193435979541));
#26023=CARTESIAN_POINT('Ctrl Pts',(1.74080458266705,1.,0.750193435979541));
#26024=CARTESIAN_POINT('Ctrl Pts',(1.74585086852298,-1.,0.751555614163629));
#26025=CARTESIAN_POINT('Ctrl Pts',(1.74585086852298,1.,0.751555614163629));
#26026=CARTESIAN_POINT('Ctrl Pts',(1.75095139468809,-1.,0.752797683531377));
#26027=CARTESIAN_POINT('Ctrl Pts',(1.75095139468809,1.,0.752797683531377));
#26028=CARTESIAN_POINT('Ctrl Pts',(1.75631083600175,-1.,0.75400925402848));
#26029=CARTESIAN_POINT('Ctrl Pts',(1.75631083600175,1.,0.75400925402848));
#26030=CARTESIAN_POINT('Ctrl Pts',(1.7619781724032,-1.,0.755220979975262));
#26031=CARTESIAN_POINT('Ctrl Pts',(1.7619781724032,1.,0.755220979975262));
#26032=CARTESIAN_POINT('Ctrl Pts',(1.76789396003141,-1.,0.756421896028403));
#26033=CARTESIAN_POINT('Ctrl Pts',(1.76789396003141,1.,0.756421896028403));
#26034=CARTESIAN_POINT('Ctrl Pts',(1.77394167108342,-1.,0.757578264077238));
#26035=CARTESIAN_POINT('Ctrl Pts',(1.77394167108342,1.,0.757578264077238));
#26036=CARTESIAN_POINT('Ctrl Pts',(1.77999411220912,-1.,0.75865062667738));
#26037=CARTESIAN_POINT('Ctrl Pts',(1.77999411220912,1.,0.75865062667738));
#26038=CARTESIAN_POINT('Ctrl Pts',(1.78596964884526,-1.,0.759614401109868));
#26039=CARTESIAN_POINT('Ctrl Pts',(1.78596964884526,1.,0.759614401109868));
#26040=CARTESIAN_POINT('Ctrl Pts',(1.79185815610802,-1.,0.760469555880425));
#26041=CARTESIAN_POINT('Ctrl Pts',(1.79185815610802,1.,0.760469555880425));
#26042=CARTESIAN_POINT('Ctrl Pts',(1.79768986997735,-1.,0.761229695230359));
#26043=CARTESIAN_POINT('Ctrl Pts',(1.79768986997735,1.,0.761229695230359));
#26044=CARTESIAN_POINT('Ctrl Pts',(1.80351583877334,-1.,0.761915336443516));
#26045=CARTESIAN_POINT('Ctrl Pts',(1.80351583877334,1.,0.761915336443516));
#26046=CARTESIAN_POINT('Ctrl Pts',(1.80938551463989,-1.,0.762546129464036));
#26047=CARTESIAN_POINT('Ctrl Pts',(1.80938551463989,1.,0.762546129464036));
#26048=CARTESIAN_POINT('Ctrl Pts',(1.81532118405566,-1.,0.763132003836783));
#26049=CARTESIAN_POINT('Ctrl Pts',(1.81532118405566,1.,0.763132003836783));
#26050=CARTESIAN_POINT('Ctrl Pts',(1.82131873145297,-1.,0.763673465462854));
#26051=CARTESIAN_POINT('Ctrl Pts',(1.82131873145297,1.,0.763673465462854));
#26052=CARTESIAN_POINT('Ctrl Pts',(1.8273599120008,-1.,0.764165902606056));
#26053=CARTESIAN_POINT('Ctrl Pts',(1.8273599120008,1.,0.764165902606056));
#26054=CARTESIAN_POINT('Ctrl Pts',(1.8334207722714,-1.,0.764602549687846));
#26055=CARTESIAN_POINT('Ctrl Pts',(1.8334207722714,1.,0.764602549687846));
#26056=CARTESIAN_POINT('Ctrl Pts',(1.83948181064823,-1.,0.764978057881688));
#26057=CARTESIAN_POINT('Ctrl Pts',(1.83948181064823,1.,0.764978057881688));
#26058=CARTESIAN_POINT('Ctrl Pts',(1.8455369887591,-1.,0.765291664861972));
#26059=CARTESIAN_POINT('Ctrl Pts',(1.8455369887591,1.,0.765291664861972));
#26060=CARTESIAN_POINT('Ctrl Pts',(1.85158945130054,-1.,0.765545710619023));
#26061=CARTESIAN_POINT('Ctrl Pts',(1.85158945130054,1.,0.765545710619023));
#26062=CARTESIAN_POINT('Ctrl Pts',(1.85764741390391,-1.,0.765744212909305));
#26063=CARTESIAN_POINT('Ctrl Pts',(1.85764741390391,1.,0.765744212909305));
#26064=CARTESIAN_POINT('Ctrl Pts',(1.86372027063314,-1.,0.765891519092557));
#26065=CARTESIAN_POINT('Ctrl Pts',(1.86372027063314,1.,0.765891519092557));
#26066=CARTESIAN_POINT('Ctrl Pts',(1.86981398314345,-1.,0.765990708546112));
#26067=CARTESIAN_POINT('Ctrl Pts',(1.86981398314345,1.,0.765990708546112));
#26068=CARTESIAN_POINT('Ctrl Pts',(1.87592888967886,-1.,0.766042837036759));
#26069=CARTESIAN_POINT('Ctrl Pts',(1.87592888967886,1.,0.766042837036759));
#26070=CARTESIAN_POINT('Ctrl Pts',(1.88206215302561,-1.,0.766047794851869));
#26071=CARTESIAN_POINT('Ctrl Pts',(1.88206215302561,1.,0.766047794851869));
#26072=CARTESIAN_POINT('Ctrl Pts',(1.88820926433409,-1.,0.76600483706209));
#26073=CARTESIAN_POINT('Ctrl Pts',(1.88820926433409,1.,0.76600483706209));
#26074=CARTESIAN_POINT('Ctrl Pts',(1.89436577771389,-1.,0.765913193856979));
#26075=CARTESIAN_POINT('Ctrl Pts',(1.89436577771389,1.,0.765913193856979));
#26076=CARTESIAN_POINT('Ctrl Pts',(1.90052930393599,-1.,0.765772772593395));
#26077=CARTESIAN_POINT('Ctrl Pts',(1.90052930393599,1.,0.765772772593395));
#26078=CARTESIAN_POINT('Ctrl Pts',(1.90669961402362,-1.,0.765584196937937));
#26079=CARTESIAN_POINT('Ctrl Pts',(1.90669961402362,1.,0.765584196937937));
#26080=CARTESIAN_POINT('Ctrl Pts',(1.91287765805174,-1.,0.765348465884739));
#26081=CARTESIAN_POINT('Ctrl Pts',(1.91287765805174,1.,0.765348465884739));
#26082=CARTESIAN_POINT('Ctrl Pts',(1.91906491634197,-1.,0.765066729667095));
#26083=CARTESIAN_POINT('Ctrl Pts',(1.91906491634197,1.,0.765066729667095));
#26084=CARTESIAN_POINT('Ctrl Pts',(1.92526263537041,-1.,0.764740025488189));
#26085=CARTESIAN_POINT('Ctrl Pts',(1.92526263537041,1.,0.764740025488189));
#26086=CARTESIAN_POINT('Ctrl Pts',(1.93147105496367,-1.,0.76436901067389));
#26087=CARTESIAN_POINT('Ctrl Pts',(1.93147105496367,1.,0.76436901067389));
#26088=CARTESIAN_POINT('Ctrl Pts',(1.93768964875867,-1.,0.763954049121394));
#26089=CARTESIAN_POINT('Ctrl Pts',(1.93768964875867,1.,0.763954049121394));
#26090=CARTESIAN_POINT('Ctrl Pts',(1.94391746617626,-1.,0.763495333538581));
#26091=CARTESIAN_POINT('Ctrl Pts',(1.94391746617626,1.,0.763495333538581));
#26092=CARTESIAN_POINT('Ctrl Pts',(1.95015342590025,-1.,0.762992990878774));
#26093=CARTESIAN_POINT('Ctrl Pts',(1.95015342590025,1.,0.762992990878774));
#26094=CARTESIAN_POINT('Ctrl Pts',(1.95639665309893,-1.,0.762447203806264));
#26095=CARTESIAN_POINT('Ctrl Pts',(1.95639665309893,1.,0.762447203806264));
#26096=CARTESIAN_POINT('Ctrl Pts',(1.96264672744229,-1.,0.761858300014575));
#26097=CARTESIAN_POINT('Ctrl Pts',(1.96264672744229,1.,0.761858300014575));
#26098=CARTESIAN_POINT('Ctrl Pts',(1.96890351582545,-1.,0.761226690483986));
#26099=CARTESIAN_POINT('Ctrl Pts',(1.96890351582545,1.,0.761226690483986));
#26100=CARTESIAN_POINT('Ctrl Pts',(1.97516705321521,-1.,0.760552825409856));
#26101=CARTESIAN_POINT('Ctrl Pts',(1.97516705321521,1.,0.760552825409856));
#26102=CARTESIAN_POINT('Ctrl Pts',(1.98143741418156,-1.,0.759837147452135));
#26103=CARTESIAN_POINT('Ctrl Pts',(1.98143741418156,1.,0.759837147452135));
#26104=CARTESIAN_POINT('Ctrl Pts',(1.98771456680806,-1.,0.759080037802243));
#26105=CARTESIAN_POINT('Ctrl Pts',(1.98771456680806,1.,0.759080037802243));
#26106=CARTESIAN_POINT('Ctrl Pts',(1.9939983109871,-1.,0.758281796766377));
#26107=CARTESIAN_POINT('Ctrl Pts',(1.9939983109871,1.,0.758281796766377));
#26108=CARTESIAN_POINT('Ctrl Pts',(2.00028834739072,-1.,0.757442676862342));
#26109=CARTESIAN_POINT('Ctrl Pts',(2.00028834739072,1.,0.757442676862342));
#26110=CARTESIAN_POINT('Ctrl Pts',(2.00658431587682,-1.,0.756562904646496));
#26111=CARTESIAN_POINT('Ctrl Pts',(2.00658431587682,1.,0.756562904646496));
#26112=CARTESIAN_POINT('Ctrl Pts',(2.01288584328149,-1.,0.755642704958101));
#26113=CARTESIAN_POINT('Ctrl Pts',(2.01288584328149,1.,0.755642704958101));
#26114=CARTESIAN_POINT('Ctrl Pts',(2.01919259406003,-1.,0.75468233072352));
#26115=CARTESIAN_POINT('Ctrl Pts',(2.01919259406003,1.,0.75468233072352));
#26116=CARTESIAN_POINT('Ctrl Pts',(2.02550428623587,-1.,0.753682061113766));
#26117=CARTESIAN_POINT('Ctrl Pts',(2.02550428623587,1.,0.753682061113766));
#26118=CARTESIAN_POINT('Ctrl Pts',(2.03182068456467,-1.,0.752642180488104));
#26119=CARTESIAN_POINT('Ctrl Pts',(2.03182068456467,1.,0.752642180488104));
#26120=CARTESIAN_POINT('Ctrl Pts',(2.03814160092173,-1.,0.751562963361384));
#26121=CARTESIAN_POINT('Ctrl Pts',(2.03814160092173,1.,0.751562963361384));
#26122=CARTESIAN_POINT('Ctrl Pts',(2.04446689147754,-1.,0.750444657874758));
#26123=CARTESIAN_POINT('Ctrl Pts',(2.04446689147754,1.,0.750444657874758));
#26124=CARTESIAN_POINT('Ctrl Pts',(2.05079645591606,-1.,0.749287468663053));
#26125=CARTESIAN_POINT('Ctrl Pts',(2.05079645591606,1.,0.749287468663053));
#26126=CARTESIAN_POINT('Ctrl Pts',(2.05713023030263,-1.,0.748091554181101));
#26127=CARTESIAN_POINT('Ctrl Pts',(2.05713023030263,1.,0.748091554181101));
#26128=CARTESIAN_POINT('Ctrl Pts',(2.06220058927162,-1.,0.747103932785504));
#26129=CARTESIAN_POINT('Ctrl Pts',(2.06220058927162,1.,0.747103932785504));
#26130=CARTESIAN_POINT('Ctrl Pts',(2.06600523016401,-1.,0.746345871542696));
#26131=CARTESIAN_POINT('Ctrl Pts',(2.06600523016401,1.,0.746345871542696));
#26132=CARTESIAN_POINT('Ctrl Pts',(2.06854248895575,-1.,0.74583279137781));
#26133=CARTESIAN_POINT('Ctrl Pts',(2.06854248895575,1.,0.74583279137781));
#26134=CARTESIAN_POINT('Ctrl Pts',(2.0698113262342,-1.,0.745574324794401));
#26135=CARTESIAN_POINT('Ctrl Pts',(2.0698113262342,1.,0.745574324794401));
#26136=CARTESIAN_POINT('',(1.60662857109684,1.,0.693717979106306));
#26137=CARTESIAN_POINT('Ctrl Pts',(1.60662857109684,1.,0.693717979106306));
#26138=CARTESIAN_POINT('Ctrl Pts',(1.61106790958151,1.,0.695712097881194));
#26139=CARTESIAN_POINT('Ctrl Pts',(1.61974673472612,1.,0.699605146405088));
#26140=CARTESIAN_POINT('Ctrl Pts',(1.63216541664676,1.,0.705159151988319));
#26141=CARTESIAN_POINT('Ctrl Pts',(1.64752408832016,1.,0.711993139355394));
#26142=CARTESIAN_POINT('Ctrl Pts',(1.6647288055568,1.,0.719585433804282));
#26143=CARTESIAN_POINT('Ctrl Pts',(1.67996158455503,1.,0.726235967997433));
#26144=CARTESIAN_POINT('Ctrl Pts',(1.69326921975743,1.,0.731963238697195));
#26145=CARTESIAN_POINT('Ctrl Pts',(1.70473309006121,1.,0.736799665724771));
#26146=CARTESIAN_POINT('Ctrl Pts',(1.71447789751927,1.,0.740795162032088));
#26147=CARTESIAN_POINT('Ctrl Pts',(1.7226822991693,1.,0.744021445433765));
#26148=CARTESIAN_POINT('Ctrl Pts',(1.72958533647399,1.,0.746574710096437));
#26149=CARTESIAN_POINT('Ctrl Pts',(1.73550351679848,1.,0.748582462954855));
#26150=CARTESIAN_POINT('Ctrl Pts',(1.74080458266705,1.,0.750193435979541));
#26151=CARTESIAN_POINT('Ctrl Pts',(1.74585086852298,1.,0.751555614163629));
#26152=CARTESIAN_POINT('Ctrl Pts',(1.75095139468809,1.,0.752797683531377));
#26153=CARTESIAN_POINT('Ctrl Pts',(1.75631083600175,1.,0.75400925402848));
#26154=CARTESIAN_POINT('Ctrl Pts',(1.7619781724032,1.,0.755220979975262));
#26155=CARTESIAN_POINT('Ctrl Pts',(1.76789396003141,1.,0.756421896028403));
#26156=CARTESIAN_POINT('Ctrl Pts',(1.77394167108342,1.,0.757578264077238));
#26157=CARTESIAN_POINT('Ctrl Pts',(1.77999411220912,1.,0.75865062667738));
#26158=CARTESIAN_POINT('Ctrl Pts',(1.78596964884526,1.,0.759614401109868));
#26159=CARTESIAN_POINT('Ctrl Pts',(1.79185815610802,1.,0.760469555880425));
#26160=CARTESIAN_POINT('Ctrl Pts',(1.79768986997735,1.,0.761229695230359));
#26161=CARTESIAN_POINT('Ctrl Pts',(1.80351583877334,1.,0.761915336443516));
#26162=CARTESIAN_POINT('Ctrl Pts',(1.80938551463989,1.,0.762546129464036));
#26163=CARTESIAN_POINT('Ctrl Pts',(1.81532118405566,1.,0.763132003836783));
#26164=CARTESIAN_POINT('Ctrl Pts',(1.82131873145297,1.,0.763673465462854));
#26165=CARTESIAN_POINT('Ctrl Pts',(1.8273599120008,1.,0.764165902606056));
#26166=CARTESIAN_POINT('Ctrl Pts',(1.8334207722714,1.,0.764602549687846));
#26167=CARTESIAN_POINT('Ctrl Pts',(1.83948181064823,1.,0.764978057881688));
#26168=CARTESIAN_POINT('Ctrl Pts',(1.8455369887591,1.,0.765291664861972));
#26169=CARTESIAN_POINT('Ctrl Pts',(1.85158945130054,1.,0.765545710619023));
#26170=CARTESIAN_POINT('Ctrl Pts',(1.85764741390391,1.,0.765744212909305));
#26171=CARTESIAN_POINT('Ctrl Pts',(1.86372027063314,1.,0.765891519092557));
#26172=CARTESIAN_POINT('Ctrl Pts',(1.86981398314345,1.,0.765990708546112));
#26173=CARTESIAN_POINT('Ctrl Pts',(1.87592888967886,1.,0.766042837036759));
#26174=CARTESIAN_POINT('Ctrl Pts',(1.88206215302561,1.,0.766047794851869));
#26175=CARTESIAN_POINT('Ctrl Pts',(1.88820926433409,1.,0.76600483706209));
#26176=CARTESIAN_POINT('Ctrl Pts',(1.89436577771389,1.,0.765913193856979));
#26177=CARTESIAN_POINT('Ctrl Pts',(1.90052930393599,1.,0.765772772593395));
#26178=CARTESIAN_POINT('Ctrl Pts',(1.90669961402362,1.,0.765584196937937));
#26179=CARTESIAN_POINT('Ctrl Pts',(1.91287765805174,1.,0.765348465884739));
#26180=CARTESIAN_POINT('Ctrl Pts',(1.91906491634197,1.,0.765066729667095));
#26181=CARTESIAN_POINT('Ctrl Pts',(1.92526263537041,1.,0.764740025488189));
#26182=CARTESIAN_POINT('Ctrl Pts',(1.93147105496367,1.,0.76436901067389));
#26183=CARTESIAN_POINT('Ctrl Pts',(1.93768964875867,1.,0.763954049121394));
#26184=CARTESIAN_POINT('Ctrl Pts',(1.94391746617626,1.,0.763495333538581));
#26185=CARTESIAN_POINT('Ctrl Pts',(1.95015342590025,1.,0.762992990878774));
#26186=CARTESIAN_POINT('Ctrl Pts',(1.95639665309893,1.,0.762447203806264));
#26187=CARTESIAN_POINT('Ctrl Pts',(1.96264672744229,1.,0.761858300014575));
#26188=CARTESIAN_POINT('Ctrl Pts',(1.96890351582545,1.,0.761226690483986));
#26189=CARTESIAN_POINT('Ctrl Pts',(1.97516705321521,1.,0.760552825409856));
#26190=CARTESIAN_POINT('Ctrl Pts',(1.98143741418156,1.,0.759837147452135));
#26191=CARTESIAN_POINT('Ctrl Pts',(1.98771456680806,1.,0.759080037802243));
#26192=CARTESIAN_POINT('Ctrl Pts',(1.9939983109871,1.,0.758281796766377));
#26193=CARTESIAN_POINT('Ctrl Pts',(2.00028834739072,1.,0.757442676862342));
#26194=CARTESIAN_POINT('Ctrl Pts',(2.00658431587682,1.,0.756562904646496));
#26195=CARTESIAN_POINT('Ctrl Pts',(2.01288584328149,1.,0.755642704958101));
#26196=CARTESIAN_POINT('Ctrl Pts',(2.01919259406003,1.,0.75468233072352));
#26197=CARTESIAN_POINT('Ctrl Pts',(2.02550428623587,1.,0.753682061113766));
#26198=CARTESIAN_POINT('Ctrl Pts',(2.03182068456467,1.,0.752642180488104));
#26199=CARTESIAN_POINT('Ctrl Pts',(2.03814160092173,1.,0.751562963361384));
#26200=CARTESIAN_POINT('Ctrl Pts',(2.04446689147754,1.,0.750444657874758));
#26201=CARTESIAN_POINT('Ctrl Pts',(2.05079645591606,1.,0.749287468663053));
#26202=CARTESIAN_POINT('Ctrl Pts',(2.05713023030263,1.,0.748091554181101));
#26203=CARTESIAN_POINT('Ctrl Pts',(2.06220058927162,1.,0.747103932785504));
#26204=CARTESIAN_POINT('Ctrl Pts',(2.06600523016401,1.,0.746345871542696));
#26205=CARTESIAN_POINT('Ctrl Pts',(2.06854248895575,1.,0.74583279137781));
#26206=CARTESIAN_POINT('Ctrl Pts',(2.0698113262342,1.,0.745574324794401));
#26207=CARTESIAN_POINT('',(1.60662857109684,0.,0.693717979106305));
#26208=CARTESIAN_POINT('Origin',(0.,0.,0.));
#26209=CARTESIAN_POINT('',(1.5055822144029,1.,0.892032620296856));
#26210=CARTESIAN_POINT('Origin',(0.,1.,0.));
#26211=CARTESIAN_POINT('',(1.5055822144029,0.,0.892032620296855));
#26212=CARTESIAN_POINT('Ctrl Pts',(1.81978687191668,-1.,1.23627494547115));
#26213=CARTESIAN_POINT('Ctrl Pts',(1.81978687191668,1.,1.23627494547115));
#26214=CARTESIAN_POINT('Ctrl Pts',(1.81925017193666,-1.,1.23509651170476));
#26215=CARTESIAN_POINT('Ctrl Pts',(1.81925017193666,1.,1.23509651170476));
#26216=CARTESIAN_POINT('Ctrl Pts',(1.81817389921279,-1.,1.2327422452705));
#26217=CARTESIAN_POINT('Ctrl Pts',(1.81817389921279,1.,1.2327422452705));
#26218=CARTESIAN_POINT('Ctrl Pts',(1.8165508718364,-1.,1.2292186489137));
#26219=CARTESIAN_POINT('Ctrl Pts',(1.8165508718364,1.,1.2292186489137));
#26220=CARTESIAN_POINT('Ctrl Pts',(1.81436959210434,-1.,1.2245361330495));
#26221=CARTESIAN_POINT('Ctrl Pts',(1.81436959210434,1.,1.2245361330495));
#26222=CARTESIAN_POINT('Ctrl Pts',(1.81161420806656,-1.,1.21870906103557));
#26223=CARTESIAN_POINT('Ctrl Pts',(1.81161420806656,1.,1.21870906103557));
#26224=CARTESIAN_POINT('Ctrl Pts',(1.80882996917129,-1.,1.21290815708314));
#26225=CARTESIAN_POINT('Ctrl Pts',(1.80882996917129,1.,1.21290815708314));
#26226=CARTESIAN_POINT('Ctrl Pts',(1.80601678480707,-1.,1.20713356605475));
#26227=CARTESIAN_POINT('Ctrl Pts',(1.80601678480707,1.,1.20713356605475));
#26228=CARTESIAN_POINT('Ctrl Pts',(1.80317454838603,-1.,1.20138548938974));
#26229=CARTESIAN_POINT('Ctrl Pts',(1.80317454838603,1.,1.20138548938974));
#26230=CARTESIAN_POINT('Ctrl Pts',(1.80030314369879,-1.,1.19566418930242));
#26231=CARTESIAN_POINT('Ctrl Pts',(1.80030314369879,1.,1.19566418930242));
#26232=CARTESIAN_POINT('Ctrl Pts',(1.79740245923478,-1.,1.18996997934445));
#26233=CARTESIAN_POINT('Ctrl Pts',(1.79740245923478,1.,1.18996997934445));
#26234=CARTESIAN_POINT('Ctrl Pts',(1.79447240321515,-1.,1.18430321697432));
#26235=CARTESIAN_POINT('Ctrl Pts',(1.79447240321515,1.,1.18430321697432));
#26236=CARTESIAN_POINT('Ctrl Pts',(1.79151291552689,-1.,1.17866429440809));
#26237=CARTESIAN_POINT('Ctrl Pts',(1.79151291552689,1.,1.17866429440809));
#26238=CARTESIAN_POINT('Ctrl Pts',(1.78852398877616,-1.,1.17305363177328));
#26239=CARTESIAN_POINT('Ctrl Pts',(1.78852398877616,1.,1.17305363177328));
#26240=CARTESIAN_POINT('Ctrl Pts',(1.78550566040443,-1.,1.16747166312303));
#26241=CARTESIAN_POINT('Ctrl Pts',(1.78550566040443,1.,1.16747166312303));
#26242=CARTESIAN_POINT('Ctrl Pts',(1.78245795881009,-1.,1.16191881298499));
#26243=CARTESIAN_POINT('Ctrl Pts',(1.78245795881009,1.,1.16191881298499));
#26244=CARTESIAN_POINT('Ctrl Pts',(1.77938085564275,-1.,1.15639547194698));
#26245=CARTESIAN_POINT('Ctrl Pts',(1.77938085564275,1.,1.15639547194698));
#26246=CARTESIAN_POINT('Ctrl Pts',(1.7762742255701,-1.,1.15090197841515));
#26247=CARTESIAN_POINT('Ctrl Pts',(1.7762742255701,1.,1.15090197841515));
#26248=CARTESIAN_POINT('Ctrl Pts',(1.77313777896194,-1.,1.1454385822692));
#26249=CARTESIAN_POINT('Ctrl Pts',(1.77313777896194,1.,1.1454385822692));
#26250=CARTESIAN_POINT('Ctrl Pts',(1.76997111386769,-1.,1.14000548336975));
#26251=CARTESIAN_POINT('Ctrl Pts',(1.76997111386769,1.,1.14000548336975));
#26252=CARTESIAN_POINT('Ctrl Pts',(1.76677384551862,-1.,1.1346029180462));
#26253=CARTESIAN_POINT('Ctrl Pts',(1.76677384551862,1.,1.1346029180462));
#26254=CARTESIAN_POINT('Ctrl Pts',(1.7635457196617,-1.,1.12923123555075));
#26255=CARTESIAN_POINT('Ctrl Pts',(1.7635457196617,1.,1.12923123555075));
#26256=CARTESIAN_POINT('Ctrl Pts',(1.76028671825096,-1.,1.12389096855086));
#26257=CARTESIAN_POINT('Ctrl Pts',(1.76028671825096,1.,1.12389096855086));
#26258=CARTESIAN_POINT('Ctrl Pts',(1.75699720772105,-1.,1.11858293216763));
#26259=CARTESIAN_POINT('Ctrl Pts',(1.75699720772105,1.,1.11858293216763));
#26260=CARTESIAN_POINT('Ctrl Pts',(1.7536777209463,-1.,1.11330807582551));
#26261=CARTESIAN_POINT('Ctrl Pts',(1.7536777209463,1.,1.11330807582551));
#26262=CARTESIAN_POINT('Ctrl Pts',(1.7503286607592,-1.,1.10806728183007));
#26263=CARTESIAN_POINT('Ctrl Pts',(1.7503286607592,1.,1.10806728183007));
#26264=CARTESIAN_POINT('Ctrl Pts',(1.74695004214923,-1.,1.10286118991143));
#26265=CARTESIAN_POINT('Ctrl Pts',(1.74695004214923,1.,1.10286118991143));
#26266=CARTESIAN_POINT('Ctrl Pts',(1.74354119236208,-1.,1.09768999241226));
#26267=CARTESIAN_POINT('Ctrl Pts',(1.74354119236208,1.,1.09768999241226));
#26268=CARTESIAN_POINT('Ctrl Pts',(1.74010053962247,-1.,1.09255329056493));
#26269=CARTESIAN_POINT('Ctrl Pts',(1.74010053962247,1.,1.09255329056493));
#26270=CARTESIAN_POINT('Ctrl Pts',(1.73662628326091,-1.,1.08745056285427));
#26271=CARTESIAN_POINT('Ctrl Pts',(1.73662628326091,1.,1.08745056285427));
#26272=CARTESIAN_POINT('Ctrl Pts',(1.73311705663407,-1.,1.08238162784749));
#26273=CARTESIAN_POINT('Ctrl Pts',(1.73311705663407,1.,1.08238162784749));
#26274=CARTESIAN_POINT('Ctrl Pts',(1.72957248977424,-1.,1.0773470373727));
#26275=CARTESIAN_POINT('Ctrl Pts',(1.72957248977424,1.,1.0773470373727));
#26276=CARTESIAN_POINT('Ctrl Pts',(1.72599406198488,-1.,1.07234866990252));
#26277=CARTESIAN_POINT('Ctrl Pts',(1.72599406198488,1.,1.07234866990252));
#26278=CARTESIAN_POINT('Ctrl Pts',(1.72238500928453,-1.,1.06738966975462));
#26279=CARTESIAN_POINT('Ctrl Pts',(1.72238500928453,1.,1.06738966975462));
#26280=CARTESIAN_POINT('Ctrl Pts',(1.71874858456904,-1.,1.06247324680647));
#26281=CARTESIAN_POINT('Ctrl Pts',(1.71874858456904,1.,1.06247324680647));
#26282=CARTESIAN_POINT('Ctrl Pts',(1.7150865442702,-1.,1.05760163192479));
#26283=CARTESIAN_POINT('Ctrl Pts',(1.7150865442702,1.,1.05760163192479));
#26284=CARTESIAN_POINT('Ctrl Pts',(1.71139783543989,-1.,1.05277517202855));
#26285=CARTESIAN_POINT('Ctrl Pts',(1.71139783543989,1.,1.05277517202855));
#26286=CARTESIAN_POINT('Ctrl Pts',(1.70767646263649,-1.,1.04799085404995));
#26287=CARTESIAN_POINT('Ctrl Pts',(1.70767646263649,1.,1.04799085404995));
#26288=CARTESIAN_POINT('Ctrl Pts',(1.70391338707982,-1.,1.04324363334554));
#26289=CARTESIAN_POINT('Ctrl Pts',(1.70391338707982,1.,1.04324363334554));
#26290=CARTESIAN_POINT('Ctrl Pts',(1.70010052930962,-1.,1.03852922490789));
#26291=CARTESIAN_POINT('Ctrl Pts',(1.70010052930962,1.,1.03852922490789));
#26292=CARTESIAN_POINT('Ctrl Pts',(1.69623414782771,-1.,1.03384646003588));
#26293=CARTESIAN_POINT('Ctrl Pts',(1.69623414782771,1.,1.03384646003588));
#26294=CARTESIAN_POINT('Ctrl Pts',(1.69231840863458,-1.,1.02919977579147));
#26295=CARTESIAN_POINT('Ctrl Pts',(1.69231840863458,1.,1.02919977579147));
#26296=CARTESIAN_POINT('Ctrl Pts',(1.68836910178447,-1.,1.02460180535255));
#26297=CARTESIAN_POINT('Ctrl Pts',(1.68836910178447,1.,1.02460180535255));
#26298=CARTESIAN_POINT('Ctrl Pts',(1.68440578021706,-1.,1.02006795074201));
#26299=CARTESIAN_POINT('Ctrl Pts',(1.68440578021706,1.,1.02006795074201));
#26300=CARTESIAN_POINT('Ctrl Pts',(1.68044289894798,-1.,1.01561026162773));
#26301=CARTESIAN_POINT('Ctrl Pts',(1.68044289894798,1.,1.01561026162773));
#26302=CARTESIAN_POINT('Ctrl Pts',(1.67648246776464,-1.,1.01123236493511));
#26303=CARTESIAN_POINT('Ctrl Pts',(1.67648246776464,1.,1.01123236493511));
#26304=CARTESIAN_POINT('Ctrl Pts',(1.67250335383293,-1.,1.00692206696414));
#26305=CARTESIAN_POINT('Ctrl Pts',(1.67250335383293,1.,1.00692206696414));
#26306=CARTESIAN_POINT('Ctrl Pts',(1.66846059277303,-1.,1.00265091003727));
#26307=CARTESIAN_POINT('Ctrl Pts',(1.66846059277303,1.,1.00265091003727));
#26308=CARTESIAN_POINT('Ctrl Pts',(1.66430758030376,-1.,0.998389654952758));
#26309=CARTESIAN_POINT('Ctrl Pts',(1.66430758030376,1.,0.998389654952758));
#26310=CARTESIAN_POINT('Ctrl Pts',(1.66001553809947,-1.,0.994121836661306));
#26311=CARTESIAN_POINT('Ctrl Pts',(1.66001553809947,1.,0.994121836661306));
#26312=CARTESIAN_POINT('Ctrl Pts',(1.65559044289699,-1.,0.989855627854165));
#26313=CARTESIAN_POINT('Ctrl Pts',(1.65559044289699,1.,0.989855627854165));
#26314=CARTESIAN_POINT('Ctrl Pts',(1.65110016612638,-1.,0.985642622920821));
#26315=CARTESIAN_POINT('Ctrl Pts',(1.65110016612638,1.,0.985642622920821));
#26316=CARTESIAN_POINT('Ctrl Pts',(1.64665139190656,-1.,0.981562530939489));
#26317=CARTESIAN_POINT('Ctrl Pts',(1.64665139190656,1.,0.981562530939489));
#26318=CARTESIAN_POINT('Ctrl Pts',(1.64233990826687,-1.,0.977689794119417));
#26319=CARTESIAN_POINT('Ctrl Pts',(1.64233990826687,1.,0.977689794119417));
#26320=CARTESIAN_POINT('Ctrl Pts',(1.63820952658144,-1.,0.974066058287419));
#26321=CARTESIAN_POINT('Ctrl Pts',(1.63820952658144,1.,0.974066058287419));
#26322=CARTESIAN_POINT('Ctrl Pts',(1.63420665729798,-1.,0.970669715997509));
#26323=CARTESIAN_POINT('Ctrl Pts',(1.63420665729798,1.,0.970669715997509));
#26324=CARTESIAN_POINT('Ctrl Pts',(1.63013849959461,-1.,0.967387853230345));
#26325=CARTESIAN_POINT('Ctrl Pts',(1.63013849959461,1.,0.967387853230345));
#26326=CARTESIAN_POINT('Ctrl Pts',(1.62571930670187,-1.,0.964046107040536));
#26327=CARTESIAN_POINT('Ctrl Pts',(1.62571930670187,1.,0.964046107040536));
#26328=CARTESIAN_POINT('Ctrl Pts',(1.62061638140221,-1.,0.960438326101729));
#26329=CARTESIAN_POINT('Ctrl Pts',(1.62061638140221,1.,0.960438326101729));
#26330=CARTESIAN_POINT('Ctrl Pts',(1.61449324337085,-1.,0.956354422920671));
#26331=CARTESIAN_POINT('Ctrl Pts',(1.61449324337085,1.,0.956354422920671));
#26332=CARTESIAN_POINT('Ctrl Pts',(1.60706069896936,-1.,0.951613284356035));
#26333=CARTESIAN_POINT('Ctrl Pts',(1.60706069896936,1.,0.951613284356035));
#26334=CARTESIAN_POINT('Ctrl Pts',(1.59810042043673,-1.,0.946078063315257));
#26335=CARTESIAN_POINT('Ctrl Pts',(1.59810042043673,1.,0.946078063315257));
#26336=CARTESIAN_POINT('Ctrl Pts',(1.58744937487176,-1.,0.939646377893399));
#26337=CARTESIAN_POINT('Ctrl Pts',(1.58744937487176,1.,0.939646377893399));
#26338=CARTESIAN_POINT('Ctrl Pts',(1.57499388382243,-1.,0.932246680108685));
#26339=CARTESIAN_POINT('Ctrl Pts',(1.57499388382243,1.,0.932246680108685));
#26340=CARTESIAN_POINT('Ctrl Pts',(1.56065988578893,-1.,0.923832188944341));
#26341=CARTESIAN_POINT('Ctrl Pts',(1.56065988578893,1.,0.923832188944341));
#26342=CARTESIAN_POINT('Ctrl Pts',(1.54440491149498,-1.,0.914375919026456));
#26343=CARTESIAN_POINT('Ctrl Pts',(1.54440491149498,1.,0.914375919026456));
#26344=CARTESIAN_POINT('Ctrl Pts',(1.52984849887993,-1.,0.905967409625651));
#26345=CARTESIAN_POINT('Ctrl Pts',(1.52984849887993,1.,0.905967409625651));
#26346=CARTESIAN_POINT('Ctrl Pts',(1.51805569590094,-1.,0.899185047483511));
#26347=CARTESIAN_POINT('Ctrl Pts',(1.51805569590094,1.,0.899185047483511));
#26348=CARTESIAN_POINT('Ctrl Pts',(1.50980486806688,-1.,0.894452006964544));
#26349=CARTESIAN_POINT('Ctrl Pts',(1.50980486806688,1.,0.894452006964544));
#26350=CARTESIAN_POINT('Ctrl Pts',(1.5055822144029,-1.,0.892032620296856));
#26351=CARTESIAN_POINT('Ctrl Pts',(1.5055822144029,1.,0.892032620296856));
#26352=CARTESIAN_POINT('',(1.81978687191668,1.,1.23627494547115));
#26353=CARTESIAN_POINT('Ctrl Pts',(1.81978687191668,1.,1.23627494547115));
#26354=CARTESIAN_POINT('Ctrl Pts',(1.81925017193666,1.,1.23509651170476));
#26355=CARTESIAN_POINT('Ctrl Pts',(1.81817389921279,1.,1.2327422452705));
#26356=CARTESIAN_POINT('Ctrl Pts',(1.8165508718364,1.,1.2292186489137));
#26357=CARTESIAN_POINT('Ctrl Pts',(1.81436959210434,1.,1.2245361330495));
#26358=CARTESIAN_POINT('Ctrl Pts',(1.81161420806656,1.,1.21870906103557));
#26359=CARTESIAN_POINT('Ctrl Pts',(1.80882996917129,1.,1.21290815708314));
#26360=CARTESIAN_POINT('Ctrl Pts',(1.80601678480707,1.,1.20713356605475));
#26361=CARTESIAN_POINT('Ctrl Pts',(1.80317454838603,1.,1.20138548938974));
#26362=CARTESIAN_POINT('Ctrl Pts',(1.80030314369879,1.,1.19566418930242));
#26363=CARTESIAN_POINT('Ctrl Pts',(1.79740245923478,1.,1.18996997934445));
#26364=CARTESIAN_POINT('Ctrl Pts',(1.79447240321515,1.,1.18430321697432));
#26365=CARTESIAN_POINT('Ctrl Pts',(1.79151291552689,1.,1.17866429440809));
#26366=CARTESIAN_POINT('Ctrl Pts',(1.78852398877616,1.,1.17305363177328));
#26367=CARTESIAN_POINT('Ctrl Pts',(1.78550566040443,1.,1.16747166312303));
#26368=CARTESIAN_POINT('Ctrl Pts',(1.78245795881009,1.,1.16191881298499));
#26369=CARTESIAN_POINT('Ctrl Pts',(1.77938085564275,1.,1.15639547194698));
#26370=CARTESIAN_POINT('Ctrl Pts',(1.7762742255701,1.,1.15090197841515));
#26371=CARTESIAN_POINT('Ctrl Pts',(1.77313777896194,1.,1.1454385822692));
#26372=CARTESIAN_POINT('Ctrl Pts',(1.76997111386769,1.,1.14000548336975));
#26373=CARTESIAN_POINT('Ctrl Pts',(1.76677384551862,1.,1.1346029180462));
#26374=CARTESIAN_POINT('Ctrl Pts',(1.7635457196617,1.,1.12923123555075));
#26375=CARTESIAN_POINT('Ctrl Pts',(1.76028671825096,1.,1.12389096855086));
#26376=CARTESIAN_POINT('Ctrl Pts',(1.75699720772105,1.,1.11858293216763));
#26377=CARTESIAN_POINT('Ctrl Pts',(1.7536777209463,1.,1.11330807582551));
#26378=CARTESIAN_POINT('Ctrl Pts',(1.7503286607592,1.,1.10806728183007));
#26379=CARTESIAN_POINT('Ctrl Pts',(1.74695004214923,1.,1.10286118991143));
#26380=CARTESIAN_POINT('Ctrl Pts',(1.74354119236208,1.,1.09768999241226));
#26381=CARTESIAN_POINT('Ctrl Pts',(1.74010053962247,1.,1.09255329056493));
#26382=CARTESIAN_POINT('Ctrl Pts',(1.73662628326091,1.,1.08745056285427));
#26383=CARTESIAN_POINT('Ctrl Pts',(1.73311705663407,1.,1.08238162784749));
#26384=CARTESIAN_POINT('Ctrl Pts',(1.72957248977424,1.,1.0773470373727));
#26385=CARTESIAN_POINT('Ctrl Pts',(1.72599406198488,1.,1.07234866990252));
#26386=CARTESIAN_POINT('Ctrl Pts',(1.72238500928453,1.,1.06738966975462));
#26387=CARTESIAN_POINT('Ctrl Pts',(1.71874858456904,1.,1.06247324680647));
#26388=CARTESIAN_POINT('Ctrl Pts',(1.7150865442702,1.,1.05760163192479));
#26389=CARTESIAN_POINT('Ctrl Pts',(1.71139783543989,1.,1.05277517202855));
#26390=CARTESIAN_POINT('Ctrl Pts',(1.70767646263649,1.,1.04799085404995));
#26391=CARTESIAN_POINT('Ctrl Pts',(1.70391338707982,1.,1.04324363334554));
#26392=CARTESIAN_POINT('Ctrl Pts',(1.70010052930962,1.,1.03852922490789));
#26393=CARTESIAN_POINT('Ctrl Pts',(1.69623414782771,1.,1.03384646003588));
#26394=CARTESIAN_POINT('Ctrl Pts',(1.69231840863458,1.,1.02919977579147));
#26395=CARTESIAN_POINT('Ctrl Pts',(1.68836910178447,1.,1.02460180535255));
#26396=CARTESIAN_POINT('Ctrl Pts',(1.68440578021706,1.,1.02006795074201));
#26397=CARTESIAN_POINT('Ctrl Pts',(1.68044289894798,1.,1.01561026162773));
#26398=CARTESIAN_POINT('Ctrl Pts',(1.67648246776464,1.,1.01123236493511));
#26399=CARTESIAN_POINT('Ctrl Pts',(1.67250335383293,1.,1.00692206696414));
#26400=CARTESIAN_POINT('Ctrl Pts',(1.66846059277303,1.,1.00265091003727));
#26401=CARTESIAN_POINT('Ctrl Pts',(1.66430758030376,1.,0.998389654952758));
#26402=CARTESIAN_POINT('Ctrl Pts',(1.66001553809947,1.,0.994121836661306));
#26403=CARTESIAN_POINT('Ctrl Pts',(1.65559044289699,1.,0.989855627854165));
#26404=CARTESIAN_POINT('Ctrl Pts',(1.65110016612638,1.,0.985642622920821));
#26405=CARTESIAN_POINT('Ctrl Pts',(1.64665139190656,1.,0.981562530939489));
#26406=CARTESIAN_POINT('Ctrl Pts',(1.64233990826687,1.,0.977689794119417));
#26407=CARTESIAN_POINT('Ctrl Pts',(1.63820952658144,1.,0.974066058287419));
#26408=CARTESIAN_POINT('Ctrl Pts',(1.63420665729798,1.,0.970669715997509));
#26409=CARTESIAN_POINT('Ctrl Pts',(1.63013849959461,1.,0.967387853230345));
#26410=CARTESIAN_POINT('Ctrl Pts',(1.62571930670187,1.,0.964046107040536));
#26411=CARTESIAN_POINT('Ctrl Pts',(1.62061638140221,1.,0.960438326101729));
#26412=CARTESIAN_POINT('Ctrl Pts',(1.61449324337085,1.,0.956354422920671));
#26413=CARTESIAN_POINT('Ctrl Pts',(1.60706069896936,1.,0.951613284356035));
#26414=CARTESIAN_POINT('Ctrl Pts',(1.59810042043673,1.,0.946078063315257));
#26415=CARTESIAN_POINT('Ctrl Pts',(1.58744937487176,1.,0.939646377893399));
#26416=CARTESIAN_POINT('Ctrl Pts',(1.57499388382243,1.,0.932246680108685));
#26417=CARTESIAN_POINT('Ctrl Pts',(1.56065988578893,1.,0.923832188944341));
#26418=CARTESIAN_POINT('Ctrl Pts',(1.54440491149498,1.,0.914375919026456));
#26419=CARTESIAN_POINT('Ctrl Pts',(1.52984849887993,1.,0.905967409625651));
#26420=CARTESIAN_POINT('Ctrl Pts',(1.51805569590094,1.,0.899185047483511));
#26421=CARTESIAN_POINT('Ctrl Pts',(1.50980486806688,1.,0.894452006964544));
#26422=CARTESIAN_POINT('Ctrl Pts',(1.5055822144029,1.,0.892032620296856));
#26423=CARTESIAN_POINT('',(1.81978687191668,0.,1.23627494547115));
#26424=CARTESIAN_POINT('Origin',(1.73811241238545,0.,1.34869019493419));
#26425=CARTESIAN_POINT('',(1.73811241238545,1.,1.34869019493419));
#26426=CARTESIAN_POINT('',(1.81978687191668,1.,1.23627494547115));
#26427=CARTESIAN_POINT('',(1.73811241238545,0.,1.34869019493419));
#26428=CARTESIAN_POINT('Ctrl Pts',(1.31362392696032,-1.,1.15624053661742));
#26429=CARTESIAN_POINT('Ctrl Pts',(1.31362392696032,1.,1.15624053661742));
#26430=CARTESIAN_POINT('Ctrl Pts',(1.31722977216397,-1.,1.15950888730809));
#26431=CARTESIAN_POINT('Ctrl Pts',(1.31722977216397,1.,1.15950888730809));
#26432=CARTESIAN_POINT('Ctrl Pts',(1.32428080721772,-1.,1.16589330093588));
#26433=CARTESIAN_POINT('Ctrl Pts',(1.32428080721772,1.,1.16589330093588));
#26434=CARTESIAN_POINT('Ctrl Pts',(1.33437539347008,-1.,1.17501305789857));
#26435=CARTESIAN_POINT('Ctrl Pts',(1.33437539347008,1.,1.17501305789857));
#26436=CARTESIAN_POINT('Ctrl Pts',(1.34687054001093,-1.,1.18625865667441));
#26437=CARTESIAN_POINT('Ctrl Pts',(1.34687054001093,1.,1.18625865667441));
#26438=CARTESIAN_POINT('Ctrl Pts',(1.36088705043885,-1.,1.1987959077932));
#26439=CARTESIAN_POINT('Ctrl Pts',(1.36088705043885,1.,1.1987959077932));
#26440=CARTESIAN_POINT('Ctrl Pts',(1.37331915607905,-1.,1.20982812925645));
#26441=CARTESIAN_POINT('Ctrl Pts',(1.37331915607905,1.,1.20982812925645));
#26442=CARTESIAN_POINT('Ctrl Pts',(1.38420564527715,-1.,1.21938737280852));
#26443=CARTESIAN_POINT('Ctrl Pts',(1.38420564527715,1.,1.21938737280852));
#26444=CARTESIAN_POINT('Ctrl Pts',(1.39361389568796,-1.,1.22752961899387));
#26445=CARTESIAN_POINT('Ctrl Pts',(1.39361389568796,1.,1.22752961899387));
#26446=CARTESIAN_POINT('Ctrl Pts',(1.40164708206106,-1.,1.23434087290423));
#26447=CARTESIAN_POINT('Ctrl Pts',(1.40164708206106,1.,1.23434087290423));
#26448=CARTESIAN_POINT('Ctrl Pts',(1.40845295531283,-1.,1.23994455029534));
#26449=CARTESIAN_POINT('Ctrl Pts',(1.40845295531283,1.,1.23994455029534));
#26450=CARTESIAN_POINT('Ctrl Pts',(1.41422913175179,-1.,1.24450600513056));
#26451=CARTESIAN_POINT('Ctrl Pts',(1.41422913175179,1.,1.24450600513056));
#26452=CARTESIAN_POINT('Ctrl Pts',(1.41923722596025,-1.,1.24824430986571));
#26453=CARTESIAN_POINT('Ctrl Pts',(1.41923722596025,1.,1.24824430986571));
#26454=CARTESIAN_POINT('Ctrl Pts',(1.42378102115575,-1.,1.2514145557001));
#26455=CARTESIAN_POINT('Ctrl Pts',(1.42378102115575,1.,1.2514145557001));
#26456=CARTESIAN_POINT('Ctrl Pts',(1.42815938799387,-1.,1.25426945222639));
#26457=CARTESIAN_POINT('Ctrl Pts',(1.42815938799387,1.,1.25426945222639));
#26458=CARTESIAN_POINT('Ctrl Pts',(1.43262645609691,-1.,1.25702687965755));
#26459=CARTESIAN_POINT('Ctrl Pts',(1.43262645609691,1.,1.25702687965755));
#26460=CARTESIAN_POINT('Ctrl Pts',(1.43734919180847,-1.,1.25983531012005));
#26461=CARTESIAN_POINT('Ctrl Pts',(1.43734919180847,1.,1.25983531012005));
#26462=CARTESIAN_POINT('Ctrl Pts',(1.44236470511303,-1.,1.26273903323859));
#26463=CARTESIAN_POINT('Ctrl Pts',(1.44236470511303,1.,1.26273903323859));
#26464=CARTESIAN_POINT('Ctrl Pts',(1.44761985001662,-1.,1.26570925118868));
#26465=CARTESIAN_POINT('Ctrl Pts',(1.44761985001662,1.,1.26570925118868));
#26466=CARTESIAN_POINT('Ctrl Pts',(1.45301422764247,-1.,1.2686778680489));
#26467=CARTESIAN_POINT('Ctrl Pts',(1.45301422764247,1.,1.2686778680489));
#26468=CARTESIAN_POINT('Ctrl Pts',(1.45843906294697,-1.,1.27156805265289));
#26469=CARTESIAN_POINT('Ctrl Pts',(1.45843906294697,1.,1.27156805265289));
#26470=CARTESIAN_POINT('Ctrl Pts',(1.46382431332476,-1.,1.27433119897822));
#26471=CARTESIAN_POINT('Ctrl Pts',(1.46382431332476,1.,1.27433119897822));
#26472=CARTESIAN_POINT('Ctrl Pts',(1.46916035917133,-1.,1.2769641483109));
#26473=CARTESIAN_POINT('Ctrl Pts',(1.46916035917133,1.,1.2769641483109));
#26474=CARTESIAN_POINT('Ctrl Pts',(1.4744717526707,-1.,1.2794891824849));
#26475=CARTESIAN_POINT('Ctrl Pts',(1.4744717526707,1.,1.2794891824849));
#26476=CARTESIAN_POINT('Ctrl Pts',(1.47980070347095,-1.,1.28194158939517));
#26477=CARTESIAN_POINT('Ctrl Pts',(1.47980070347095,1.,1.28194158939517));
#26478=CARTESIAN_POINT('Ctrl Pts',(1.4851881711891,-1.,1.28435533880201));
#26479=CARTESIAN_POINT('Ctrl Pts',(1.4851881711891,1.,1.28435533880201));
#26480=CARTESIAN_POINT('Ctrl Pts',(1.4906522831278,-1.,1.2867467611644));
#26481=CARTESIAN_POINT('Ctrl Pts',(1.4906522831278,1.,1.2867467611644));
#26482=CARTESIAN_POINT('Ctrl Pts',(1.49618896881754,-1.,1.28911506584254));
#26483=CARTESIAN_POINT('Ctrl Pts',(1.49618896881754,1.,1.28911506584254));
#26484=CARTESIAN_POINT('Ctrl Pts',(1.50178230149776,-1.,1.29145022885181));
#26485=CARTESIAN_POINT('Ctrl Pts',(1.50178230149776,1.,1.29145022885181));
#26486=CARTESIAN_POINT('Ctrl Pts',(1.50741159078365,-1.,1.29373841372842));
#26487=CARTESIAN_POINT('Ctrl Pts',(1.50741159078365,1.,1.29373841372842));
#26488=CARTESIAN_POINT('Ctrl Pts',(1.51305994241402,-1.,1.29596850710509));
#26489=CARTESIAN_POINT('Ctrl Pts',(1.51305994241402,1.,1.29596850710509));
#26490=CARTESIAN_POINT('Ctrl Pts',(1.51872184912724,-1.,1.29813791800747));
#26491=CARTESIAN_POINT('Ctrl Pts',(1.51872184912724,1.,1.29813791800747));
#26492=CARTESIAN_POINT('Ctrl Pts',(1.52439957861062,-1.,1.30024984366328));
#26493=CARTESIAN_POINT('Ctrl Pts',(1.52439957861062,1.,1.30024984366328));
#26494=CARTESIAN_POINT('Ctrl Pts',(1.53009970283891,-1.,1.30231064395568));
#26495=CARTESIAN_POINT('Ctrl Pts',(1.53009970283891,1.,1.30231064395568));
#26496=CARTESIAN_POINT('Ctrl Pts',(1.53582981268977,-1.,1.30432735639489));
#26497=CARTESIAN_POINT('Ctrl Pts',(1.53582981268977,1.,1.30432735639489));
#26498=CARTESIAN_POINT('Ctrl Pts',(1.54159462645432,-1.,1.30630475189556));
#26499=CARTESIAN_POINT('Ctrl Pts',(1.54159462645432,1.,1.30630475189556));
#26500=CARTESIAN_POINT('Ctrl Pts',(1.54739413957185,-1.,1.30824393907473));
#26501=CARTESIAN_POINT('Ctrl Pts',(1.54739413957185,1.,1.30824393907473));
#26502=CARTESIAN_POINT('Ctrl Pts',(1.55322568759481,-1.,1.31014393684222));
#26503=CARTESIAN_POINT('Ctrl Pts',(1.55322568759481,1.,1.31014393684222));
#26504=CARTESIAN_POINT('Ctrl Pts',(1.55908521254821,-1.,1.31200264341696));
#26505=CARTESIAN_POINT('Ctrl Pts',(1.55908521254821,1.,1.31200264341696));
#26506=CARTESIAN_POINT('Ctrl Pts',(1.56496872402353,-1.,1.31381795281002));
#26507=CARTESIAN_POINT('Ctrl Pts',(1.56496872402353,1.,1.31381795281002));
#26508=CARTESIAN_POINT('Ctrl Pts',(1.57087397835723,-1.,1.31558903860016));
#26509=CARTESIAN_POINT('Ctrl Pts',(1.57087397835723,1.,1.31558903860016));
#26510=CARTESIAN_POINT('Ctrl Pts',(1.5768005650559,-1.,1.31731642317187));
#26511=CARTESIAN_POINT('Ctrl Pts',(1.5768005650559,1.,1.31731642317187));
#26512=CARTESIAN_POINT('Ctrl Pts',(1.58274907898834,-1.,1.31900135021432));
#26513=CARTESIAN_POINT('Ctrl Pts',(1.58274907898834,1.,1.31900135021432));
#26514=CARTESIAN_POINT('Ctrl Pts',(1.58872057258245,-1.,1.32064537110892));
#26515=CARTESIAN_POINT('Ctrl Pts',(1.58872057258245,1.,1.32064537110892));
#26516=CARTESIAN_POINT('Ctrl Pts',(1.59471591079403,-1.,1.32224985747682));
#26517=CARTESIAN_POINT('Ctrl Pts',(1.59471591079403,1.,1.32224985747682));
#26518=CARTESIAN_POINT('Ctrl Pts',(1.60073511858687,-1.,1.32381550858256));
#26519=CARTESIAN_POINT('Ctrl Pts',(1.60073511858687,1.,1.32381550858256));
#26520=CARTESIAN_POINT('Ctrl Pts',(1.60677758290954,-1.,1.32534250785782));
#26521=CARTESIAN_POINT('Ctrl Pts',(1.60677758290954,1.,1.32534250785782));
#26522=CARTESIAN_POINT('Ctrl Pts',(1.6128423401575,-1.,1.32683074483356));
#26523=CARTESIAN_POINT('Ctrl Pts',(1.6128423401575,1.,1.32683074483356));
#26524=CARTESIAN_POINT('Ctrl Pts',(1.61892832270724,-1.,1.32828000610449));
#26525=CARTESIAN_POINT('Ctrl Pts',(1.61892832270724,1.,1.32828000610449));
#26526=CARTESIAN_POINT('Ctrl Pts',(1.62503464209797,-1.,1.3296901950568));
#26527=CARTESIAN_POINT('Ctrl Pts',(1.62503464209797,1.,1.3296901950568));
#26528=CARTESIAN_POINT('Ctrl Pts',(1.63116079730923,-1.,1.33106149345645));
#26529=CARTESIAN_POINT('Ctrl Pts',(1.63116079730923,1.,1.33106149345645));
#26530=CARTESIAN_POINT('Ctrl Pts',(1.63730653475089,-1.,1.33239425103724));
#26531=CARTESIAN_POINT('Ctrl Pts',(1.63730653475089,1.,1.33239425103724));
#26532=CARTESIAN_POINT('Ctrl Pts',(1.6434717485603,-1.,1.33368890676572));
#26533=CARTESIAN_POINT('Ctrl Pts',(1.6434717485603,1.,1.33368890676572));
#26534=CARTESIAN_POINT('Ctrl Pts',(1.6496563728683,-1.,1.33494590467993));
#26535=CARTESIAN_POINT('Ctrl Pts',(1.6496563728683,1.,1.33494590467993));
#26536=CARTESIAN_POINT('Ctrl Pts',(1.65586025952593,-1.,1.33616559745172));
#26537=CARTESIAN_POINT('Ctrl Pts',(1.65586025952593,1.,1.33616559745172));
#26538=CARTESIAN_POINT('Ctrl Pts',(1.66208312541983,-1.,1.33734820885262));
#26539=CARTESIAN_POINT('Ctrl Pts',(1.66208312541983,1.,1.33734820885262));
#26540=CARTESIAN_POINT('Ctrl Pts',(1.66832460783989,-1.,1.33849388654388));
#26541=CARTESIAN_POINT('Ctrl Pts',(1.66832460783989,1.,1.33849388654388));
#26542=CARTESIAN_POINT('Ctrl Pts',(1.67458429426086,-1.,1.3396027347034));
#26543=CARTESIAN_POINT('Ctrl Pts',(1.67458429426086,1.,1.3396027347034));
#26544=CARTESIAN_POINT('Ctrl Pts',(1.68086176030362,-1.,1.34067485185203));
#26545=CARTESIAN_POINT('Ctrl Pts',(1.68086176030362,1.,1.34067485185203));
#26546=CARTESIAN_POINT('Ctrl Pts',(1.68715660868764,-1.,1.341710374848));
#26547=CARTESIAN_POINT('Ctrl Pts',(1.68715660868764,1.,1.341710374848));
#26548=CARTESIAN_POINT('Ctrl Pts',(1.6934684849687,-1.,1.34270948206319));
#26549=CARTESIAN_POINT('Ctrl Pts',(1.6934684849687,1.,1.34270948206319));
#26550=CARTESIAN_POINT('Ctrl Pts',(1.69979707754427,-1.,1.34367237124483));
#26551=CARTESIAN_POINT('Ctrl Pts',(1.69979707754427,1.,1.34367237124483));
#26552=CARTESIAN_POINT('Ctrl Pts',(1.70614212266738,-1.,1.34459924533831));
#26553=CARTESIAN_POINT('Ctrl Pts',(1.70614212266738,1.,1.34459924533831));
#26554=CARTESIAN_POINT('Ctrl Pts',(1.71250340686822,-1.,1.34549029589416));
#26555=CARTESIAN_POINT('Ctrl Pts',(1.71250340686822,1.,1.34549029589416));
#26556=CARTESIAN_POINT('Ctrl Pts',(1.7188807715049,-1.,1.34634568653227));
#26557=CARTESIAN_POINT('Ctrl Pts',(1.7188807715049,1.,1.34634568653227));
#26558=CARTESIAN_POINT('Ctrl Pts',(1.72527410680674,-1.,1.34716554819527));
#26559=CARTESIAN_POINT('Ctrl Pts',(1.72527410680674,1.,1.34716554819527));
#26560=CARTESIAN_POINT('Ctrl Pts',(1.7304014965394,-1.,1.34779309152035));
#26561=CARTESIAN_POINT('Ctrl Pts',(1.7304014965394,1.,1.34779309152035));
#26562=CARTESIAN_POINT('Ctrl Pts',(1.73425417885907,-1.,1.34824783112887));
#26563=CARTESIAN_POINT('Ctrl Pts',(1.73425417885907,1.,1.34824783112887));
#26564=CARTESIAN_POINT('Ctrl Pts',(1.73682580585691,-1.,1.34854391898045));
#26565=CARTESIAN_POINT('Ctrl Pts',(1.73682580585691,1.,1.34854391898045));
#26566=CARTESIAN_POINT('Ctrl Pts',(1.73811241238545,-1.,1.34869019493419));
#26567=CARTESIAN_POINT('Ctrl Pts',(1.73811241238545,1.,1.34869019493419));
#26568=CARTESIAN_POINT('',(1.31362392696032,1.,1.15624053661742));
#26569=CARTESIAN_POINT('Ctrl Pts',(1.31362392696032,1.,1.15624053661742));
#26570=CARTESIAN_POINT('Ctrl Pts',(1.31722977216397,1.,1.15950888730809));
#26571=CARTESIAN_POINT('Ctrl Pts',(1.32428080721772,1.,1.16589330093588));
#26572=CARTESIAN_POINT('Ctrl Pts',(1.33437539347008,1.,1.17501305789857));
#26573=CARTESIAN_POINT('Ctrl Pts',(1.34687054001093,1.,1.18625865667441));
#26574=CARTESIAN_POINT('Ctrl Pts',(1.36088705043885,1.,1.1987959077932));
#26575=CARTESIAN_POINT('Ctrl Pts',(1.37331915607905,1.,1.20982812925645));
#26576=CARTESIAN_POINT('Ctrl Pts',(1.38420564527715,1.,1.21938737280852));
#26577=CARTESIAN_POINT('Ctrl Pts',(1.39361389568796,1.,1.22752961899387));
#26578=CARTESIAN_POINT('Ctrl Pts',(1.40164708206106,1.,1.23434087290423));
#26579=CARTESIAN_POINT('Ctrl Pts',(1.40845295531283,1.,1.23994455029534));
#26580=CARTESIAN_POINT('Ctrl Pts',(1.41422913175179,1.,1.24450600513056));
#26581=CARTESIAN_POINT('Ctrl Pts',(1.41923722596025,1.,1.24824430986571));
#26582=CARTESIAN_POINT('Ctrl Pts',(1.42378102115575,1.,1.2514145557001));
#26583=CARTESIAN_POINT('Ctrl Pts',(1.42815938799387,1.,1.25426945222639));
#26584=CARTESIAN_POINT('Ctrl Pts',(1.43262645609691,1.,1.25702687965755));
#26585=CARTESIAN_POINT('Ctrl Pts',(1.43734919180847,1.,1.25983531012005));
#26586=CARTESIAN_POINT('Ctrl Pts',(1.44236470511303,1.,1.26273903323859));
#26587=CARTESIAN_POINT('Ctrl Pts',(1.44761985001662,1.,1.26570925118868));
#26588=CARTESIAN_POINT('Ctrl Pts',(1.45301422764247,1.,1.2686778680489));
#26589=CARTESIAN_POINT('Ctrl Pts',(1.45843906294697,1.,1.27156805265289));
#26590=CARTESIAN_POINT('Ctrl Pts',(1.46382431332476,1.,1.27433119897822));
#26591=CARTESIAN_POINT('Ctrl Pts',(1.46916035917133,1.,1.2769641483109));
#26592=CARTESIAN_POINT('Ctrl Pts',(1.4744717526707,1.,1.2794891824849));
#26593=CARTESIAN_POINT('Ctrl Pts',(1.47980070347095,1.,1.28194158939517));
#26594=CARTESIAN_POINT('Ctrl Pts',(1.4851881711891,1.,1.28435533880201));
#26595=CARTESIAN_POINT('Ctrl Pts',(1.4906522831278,1.,1.2867467611644));
#26596=CARTESIAN_POINT('Ctrl Pts',(1.49618896881754,1.,1.28911506584254));
#26597=CARTESIAN_POINT('Ctrl Pts',(1.50178230149776,1.,1.29145022885181));
#26598=CARTESIAN_POINT('Ctrl Pts',(1.50741159078365,1.,1.29373841372842));
#26599=CARTESIAN_POINT('Ctrl Pts',(1.51305994241402,1.,1.29596850710509));
#26600=CARTESIAN_POINT('Ctrl Pts',(1.51872184912724,1.,1.29813791800747));
#26601=CARTESIAN_POINT('Ctrl Pts',(1.52439957861062,1.,1.30024984366328));
#26602=CARTESIAN_POINT('Ctrl Pts',(1.53009970283891,1.,1.30231064395568));
#26603=CARTESIAN_POINT('Ctrl Pts',(1.53582981268977,1.,1.30432735639489));
#26604=CARTESIAN_POINT('Ctrl Pts',(1.54159462645432,1.,1.30630475189556));
#26605=CARTESIAN_POINT('Ctrl Pts',(1.54739413957185,1.,1.30824393907473));
#26606=CARTESIAN_POINT('Ctrl Pts',(1.55322568759481,1.,1.31014393684222));
#26607=CARTESIAN_POINT('Ctrl Pts',(1.55908521254821,1.,1.31200264341696));
#26608=CARTESIAN_POINT('Ctrl Pts',(1.56496872402353,1.,1.31381795281002));
#26609=CARTESIAN_POINT('Ctrl Pts',(1.57087397835723,1.,1.31558903860016));
#26610=CARTESIAN_POINT('Ctrl Pts',(1.5768005650559,1.,1.31731642317187));
#26611=CARTESIAN_POINT('Ctrl Pts',(1.58274907898834,1.,1.31900135021432));
#26612=CARTESIAN_POINT('Ctrl Pts',(1.58872057258245,1.,1.32064537110892));
#26613=CARTESIAN_POINT('Ctrl Pts',(1.59471591079403,1.,1.32224985747682));
#26614=CARTESIAN_POINT('Ctrl Pts',(1.60073511858687,1.,1.32381550858256));
#26615=CARTESIAN_POINT('Ctrl Pts',(1.60677758290954,1.,1.32534250785782));
#26616=CARTESIAN_POINT('Ctrl Pts',(1.6128423401575,1.,1.32683074483356));
#26617=CARTESIAN_POINT('Ctrl Pts',(1.61892832270724,1.,1.32828000610449));
#26618=CARTESIAN_POINT('Ctrl Pts',(1.62503464209797,1.,1.3296901950568));
#26619=CARTESIAN_POINT('Ctrl Pts',(1.63116079730923,1.,1.33106149345645));
#26620=CARTESIAN_POINT('Ctrl Pts',(1.63730653475089,1.,1.33239425103724));
#26621=CARTESIAN_POINT('Ctrl Pts',(1.6434717485603,1.,1.33368890676572));
#26622=CARTESIAN_POINT('Ctrl Pts',(1.6496563728683,1.,1.33494590467993));
#26623=CARTESIAN_POINT('Ctrl Pts',(1.65586025952593,1.,1.33616559745172));
#26624=CARTESIAN_POINT('Ctrl Pts',(1.66208312541983,1.,1.33734820885262));
#26625=CARTESIAN_POINT('Ctrl Pts',(1.66832460783989,1.,1.33849388654388));
#26626=CARTESIAN_POINT('Ctrl Pts',(1.67458429426086,1.,1.3396027347034));
#26627=CARTESIAN_POINT('Ctrl Pts',(1.68086176030362,1.,1.34067485185203));
#26628=CARTESIAN_POINT('Ctrl Pts',(1.68715660868764,1.,1.341710374848));
#26629=CARTESIAN_POINT('Ctrl Pts',(1.6934684849687,1.,1.34270948206319));
#26630=CARTESIAN_POINT('Ctrl Pts',(1.69979707754427,1.,1.34367237124483));
#26631=CARTESIAN_POINT('Ctrl Pts',(1.70614212266738,1.,1.34459924533831));
#26632=CARTESIAN_POINT('Ctrl Pts',(1.71250340686822,1.,1.34549029589416));
#26633=CARTESIAN_POINT('Ctrl Pts',(1.7188807715049,1.,1.34634568653227));
#26634=CARTESIAN_POINT('Ctrl Pts',(1.72527410680674,1.,1.34716554819527));
#26635=CARTESIAN_POINT('Ctrl Pts',(1.7304014965394,1.,1.34779309152035));
#26636=CARTESIAN_POINT('Ctrl Pts',(1.73425417885907,1.,1.34824783112887));
#26637=CARTESIAN_POINT('Ctrl Pts',(1.73682580585691,1.,1.34854391898045));
#26638=CARTESIAN_POINT('Ctrl Pts',(1.73811241238545,1.,1.34869019493419));
#26639=CARTESIAN_POINT('',(1.31362392696032,0.,1.15624053661742));
#26640=CARTESIAN_POINT('Origin',(0.,0.,0.));
#26641=CARTESIAN_POINT('',(1.15624053661742,1.,1.31362392696033));
#26642=CARTESIAN_POINT('Origin',(0.,1.,0.));
#26643=CARTESIAN_POINT('',(1.15624053661742,0.,1.31362392696032));
#26644=CARTESIAN_POINT('Ctrl Pts',(1.34869019493419,-1.,1.73811241238545));
#26645=CARTESIAN_POINT('Ctrl Pts',(1.34869019493419,1.,1.73811241238545));
#26646=CARTESIAN_POINT('Ctrl Pts',(1.34854391898145,-1.,1.73682580585819));
#26647=CARTESIAN_POINT('Ctrl Pts',(1.34854391898145,1.,1.73682580585819));
#26648=CARTESIAN_POINT('Ctrl Pts',(1.34824783113158,-1.,1.73425417886255));
#26649=CARTESIAN_POINT('Ctrl Pts',(1.34824783113158,1.,1.73425417886255));
#26650=CARTESIAN_POINT('Ctrl Pts',(1.3477930915247,-1.,1.73040149654497));
#26651=CARTESIAN_POINT('Ctrl Pts',(1.3477930915247,1.,1.73040149654497));
#26652=CARTESIAN_POINT('Ctrl Pts',(1.34716554820013,-1.,1.72527410681298));
#26653=CARTESIAN_POINT('Ctrl Pts',(1.34716554820013,1.,1.72527410681298));
#26654=CARTESIAN_POINT('Ctrl Pts',(1.34634568653586,-1.,1.7188807715095));
#26655=CARTESIAN_POINT('Ctrl Pts',(1.34634568653586,1.,1.7188807715095));
#26656=CARTESIAN_POINT('Ctrl Pts',(1.34549029589563,-1.,1.71250340687011));
#26657=CARTESIAN_POINT('Ctrl Pts',(1.34549029589563,1.,1.71250340687011));
#26658=CARTESIAN_POINT('Ctrl Pts',(1.34459924533783,-1.,1.70614212266676));
#26659=CARTESIAN_POINT('Ctrl Pts',(1.34459924533783,1.,1.70614212266676));
#26660=CARTESIAN_POINT('Ctrl Pts',(1.34367237124322,-1.,1.69979707754221));
#26661=CARTESIAN_POINT('Ctrl Pts',(1.34367237124322,1.,1.69979707754221));
#26662=CARTESIAN_POINT('Ctrl Pts',(1.34270948206139,-1.,1.6934684849664));
#26663=CARTESIAN_POINT('Ctrl Pts',(1.34270948206139,1.,1.6934684849664));
#26664=CARTESIAN_POINT('Ctrl Pts',(1.34171037484673,-1.,1.68715660868602));
#26665=CARTESIAN_POINT('Ctrl Pts',(1.34171037484673,1.,1.68715660868602));
#26666=CARTESIAN_POINT('Ctrl Pts',(1.3406748518516,-1.,1.68086176030308));
#26667=CARTESIAN_POINT('Ctrl Pts',(1.3406748518516,1.,1.68086176030308));
#26668=CARTESIAN_POINT('Ctrl Pts',(1.33960273470372,-1.,1.67458429426126));
#26669=CARTESIAN_POINT('Ctrl Pts',(1.33960273470372,1.,1.67458429426126));
#26670=CARTESIAN_POINT('Ctrl Pts',(1.33849388654458,-1.,1.66832460784078));
#26671=CARTESIAN_POINT('Ctrl Pts',(1.33849388654458,1.,1.66832460784078));
#26672=CARTESIAN_POINT('Ctrl Pts',(1.33734820885331,-1.,1.66208312542073));
#26673=CARTESIAN_POINT('Ctrl Pts',(1.33734820885331,1.,1.66208312542073));
#26674=CARTESIAN_POINT('Ctrl Pts',(1.33616559745217,-1.,1.65586025952651));
#26675=CARTESIAN_POINT('Ctrl Pts',(1.33616559745217,1.,1.65586025952651));
#26676=CARTESIAN_POINT('Ctrl Pts',(1.33494590468003,-1.,1.64965637286843));
#26677=CARTESIAN_POINT('Ctrl Pts',(1.33494590468003,1.,1.64965637286843));
#26678=CARTESIAN_POINT('Ctrl Pts',(1.33368890676554,-1.,1.64347174856007));
#26679=CARTESIAN_POINT('Ctrl Pts',(1.33368890676554,1.,1.64347174856007));
#26680=CARTESIAN_POINT('Ctrl Pts',(1.33239425103694,-1.,1.6373065347505));
#26681=CARTESIAN_POINT('Ctrl Pts',(1.33239425103694,1.,1.6373065347505));
#26682=CARTESIAN_POINT('Ctrl Pts',(1.33106149345618,-1.,1.63116079730887));
#26683=CARTESIAN_POINT('Ctrl Pts',(1.33106149345618,1.,1.63116079730887));
#26684=CARTESIAN_POINT('Ctrl Pts',(1.32969019505665,-1.,1.62503464209777));
#26685=CARTESIAN_POINT('Ctrl Pts',(1.32969019505665,1.,1.62503464209777));
#26686=CARTESIAN_POINT('Ctrl Pts',(1.32828000610448,-1.,1.61892832270723));
#26687=CARTESIAN_POINT('Ctrl Pts',(1.32828000610448,1.,1.61892832270723));
#26688=CARTESIAN_POINT('Ctrl Pts',(1.32683074483365,-1.,1.61284234015762));
#26689=CARTESIAN_POINT('Ctrl Pts',(1.32683074483365,1.,1.61284234015762));
#26690=CARTESIAN_POINT('Ctrl Pts',(1.32534250785794,-1.,1.6067775829097));
#26691=CARTESIAN_POINT('Ctrl Pts',(1.32534250785794,1.,1.6067775829097));
#26692=CARTESIAN_POINT('Ctrl Pts',(1.32381550858266,-1.,1.600735118587));
#26693=CARTESIAN_POINT('Ctrl Pts',(1.32381550858266,1.,1.600735118587));
#26694=CARTESIAN_POINT('Ctrl Pts',(1.32224985747686,-1.,1.59471591079408));
#26695=CARTESIAN_POINT('Ctrl Pts',(1.32224985747686,1.,1.59471591079408));
#26696=CARTESIAN_POINT('Ctrl Pts',(1.32064537110891,-1.,1.58872057258244));
#26697=CARTESIAN_POINT('Ctrl Pts',(1.32064537110891,1.,1.58872057258244));
#26698=CARTESIAN_POINT('Ctrl Pts',(1.31900135021428,-1.,1.58274907898829));
#26699=CARTESIAN_POINT('Ctrl Pts',(1.31900135021428,1.,1.58274907898829));
#26700=CARTESIAN_POINT('Ctrl Pts',(1.31731642317183,-1.,1.57680056505585));
#26701=CARTESIAN_POINT('Ctrl Pts',(1.31731642317183,1.,1.57680056505585));
#26702=CARTESIAN_POINT('Ctrl Pts',(1.31558903860015,-1.,1.57087397835721));
#26703=CARTESIAN_POINT('Ctrl Pts',(1.31558903860015,1.,1.57087397835721));
#26704=CARTESIAN_POINT('Ctrl Pts',(1.31381795281002,-1.,1.56496872402352));
#26705=CARTESIAN_POINT('Ctrl Pts',(1.31381795281002,1.,1.56496872402352));
#26706=CARTESIAN_POINT('Ctrl Pts',(1.31200264341696,-1.,1.55908521254822));
#26707=CARTESIAN_POINT('Ctrl Pts',(1.31200264341696,1.,1.55908521254822));
#26708=CARTESIAN_POINT('Ctrl Pts',(1.31014393684221,-1.,1.55322568759481));
#26709=CARTESIAN_POINT('Ctrl Pts',(1.31014393684221,1.,1.55322568759481));
#26710=CARTESIAN_POINT('Ctrl Pts',(1.30824393907471,-1.,1.54739413957183));
#26711=CARTESIAN_POINT('Ctrl Pts',(1.30824393907471,1.,1.54739413957183));
#26712=CARTESIAN_POINT('Ctrl Pts',(1.30630475189553,-1.,1.54159462645428));
#26713=CARTESIAN_POINT('Ctrl Pts',(1.30630475189553,1.,1.54159462645428));
#26714=CARTESIAN_POINT('Ctrl Pts',(1.30432735639487,-1.,1.53582981268976));
#26715=CARTESIAN_POINT('Ctrl Pts',(1.30432735639487,1.,1.53582981268976));
#26716=CARTESIAN_POINT('Ctrl Pts',(1.3023106439557,-1.,1.53009970283893));
#26717=CARTESIAN_POINT('Ctrl Pts',(1.3023106439557,1.,1.53009970283893));
#26718=CARTESIAN_POINT('Ctrl Pts',(1.30024984366334,-1.,1.5243995786107));
#26719=CARTESIAN_POINT('Ctrl Pts',(1.30024984366334,1.,1.5243995786107));
#26720=CARTESIAN_POINT('Ctrl Pts',(1.29813791800757,-1.,1.51872184912735));
#26721=CARTESIAN_POINT('Ctrl Pts',(1.29813791800757,1.,1.51872184912735));
#26722=CARTESIAN_POINT('Ctrl Pts',(1.29596850710518,-1.,1.51305994241412));
#26723=CARTESIAN_POINT('Ctrl Pts',(1.29596850710518,1.,1.51305994241412));
#26724=CARTESIAN_POINT('Ctrl Pts',(1.29373841372843,-1.,1.50741159078367));
#26725=CARTESIAN_POINT('Ctrl Pts',(1.29373841372843,1.,1.50741159078367));
#26726=CARTESIAN_POINT('Ctrl Pts',(1.29145022885171,-1.,1.50178230149764));
#26727=CARTESIAN_POINT('Ctrl Pts',(1.29145022885171,1.,1.50178230149764));
#26728=CARTESIAN_POINT('Ctrl Pts',(1.28911506584232,-1.,1.49618896881729));
#26729=CARTESIAN_POINT('Ctrl Pts',(1.28911506584232,1.,1.49618896881729));
#26730=CARTESIAN_POINT('Ctrl Pts',(1.28674676116415,-1.,1.4906522831275));
#26731=CARTESIAN_POINT('Ctrl Pts',(1.28674676116415,1.,1.4906522831275));
#26732=CARTESIAN_POINT('Ctrl Pts',(1.28435533880184,-1.,1.48518817118891));
#26733=CARTESIAN_POINT('Ctrl Pts',(1.28435533880184,1.,1.48518817118891));
#26734=CARTESIAN_POINT('Ctrl Pts',(1.28194158939522,-1.,1.47980070347102));
#26735=CARTESIAN_POINT('Ctrl Pts',(1.28194158939522,1.,1.47980070347102));
#26736=CARTESIAN_POINT('Ctrl Pts',(1.27948918248524,-1.,1.4744717526711));
#26737=CARTESIAN_POINT('Ctrl Pts',(1.27948918248524,1.,1.4744717526711));
#26738=CARTESIAN_POINT('Ctrl Pts',(1.27696414831144,-1.,1.46916035917197));
#26739=CARTESIAN_POINT('Ctrl Pts',(1.27696414831144,1.,1.46916035917197));
#26740=CARTESIAN_POINT('Ctrl Pts',(1.27433119897877,-1.,1.4638243133254));
#26741=CARTESIAN_POINT('Ctrl Pts',(1.27433119897877,1.,1.4638243133254));
#26742=CARTESIAN_POINT('Ctrl Pts',(1.27156805265312,-1.,1.45843906294725));
#26743=CARTESIAN_POINT('Ctrl Pts',(1.27156805265312,1.,1.45843906294725));
#26744=CARTESIAN_POINT('Ctrl Pts',(1.26867786804854,-1.,1.45301422764205));
#26745=CARTESIAN_POINT('Ctrl Pts',(1.26867786804854,1.,1.45301422764205));
#26746=CARTESIAN_POINT('Ctrl Pts',(1.26570925118767,-1.,1.44761985001544));
#26747=CARTESIAN_POINT('Ctrl Pts',(1.26570925118767,1.,1.44761985001544));
#26748=CARTESIAN_POINT('Ctrl Pts',(1.26273903323723,-1.,1.44236470511145));
#26749=CARTESIAN_POINT('Ctrl Pts',(1.26273903323723,1.,1.44236470511145));
#26750=CARTESIAN_POINT('Ctrl Pts',(1.25983531011894,-1.,1.43734919180719));
#26751=CARTESIAN_POINT('Ctrl Pts',(1.25983531011894,1.,1.43734919180719));
#26752=CARTESIAN_POINT('Ctrl Pts',(1.25702687965744,-1.,1.43262645609679));
#26753=CARTESIAN_POINT('Ctrl Pts',(1.25702687965744,1.,1.43262645609679));
#26754=CARTESIAN_POINT('Ctrl Pts',(1.25426945222783,-1.,1.42815938799555));
#26755=CARTESIAN_POINT('Ctrl Pts',(1.25426945222783,1.,1.42815938799555));
#26756=CARTESIAN_POINT('Ctrl Pts',(1.25141455570299,-1.,1.42378102115911));
#26757=CARTESIAN_POINT('Ctrl Pts',(1.25141455570299,1.,1.42378102115911));
#26758=CARTESIAN_POINT('Ctrl Pts',(1.24824430986911,-1.,1.41923722596421));
#26759=CARTESIAN_POINT('Ctrl Pts',(1.24824430986911,1.,1.41923722596421));
#26760=CARTESIAN_POINT('Ctrl Pts',(1.24450600513278,-1.,1.41422913175437));
#26761=CARTESIAN_POINT('Ctrl Pts',(1.24450600513278,1.,1.41422913175437));
#26762=CARTESIAN_POINT('Ctrl Pts',(1.23994455029421,-1.,1.40845295531151));
#26763=CARTESIAN_POINT('Ctrl Pts',(1.23994455029421,1.,1.40845295531151));
#26764=CARTESIAN_POINT('Ctrl Pts',(1.23434087289768,-1.,1.40164708205345));
#26765=CARTESIAN_POINT('Ctrl Pts',(1.23434087289768,1.,1.40164708205345));
#26766=CARTESIAN_POINT('Ctrl Pts',(1.22752961898063,-1.,1.39361389567257));
#26767=CARTESIAN_POINT('Ctrl Pts',(1.22752961898063,1.,1.39361389567257));
#26768=CARTESIAN_POINT('Ctrl Pts',(1.21938737278853,-1.,1.38420564525391));
#26769=CARTESIAN_POINT('Ctrl Pts',(1.21938737278853,1.,1.38420564525391));
#26770=CARTESIAN_POINT('Ctrl Pts',(1.20982812923113,-1.,1.37331915604962));
#26771=CARTESIAN_POINT('Ctrl Pts',(1.20982812923113,1.,1.37331915604962));
#26772=CARTESIAN_POINT('Ctrl Pts',(1.1987959077656,-1.,1.36088705040677));
#26773=CARTESIAN_POINT('Ctrl Pts',(1.1987959077656,1.,1.36088705040677));
#26774=CARTESIAN_POINT('Ctrl Pts',(1.18625865664915,-1.,1.34687053998157));
#26775=CARTESIAN_POINT('Ctrl Pts',(1.18625865664915,1.,1.34687053998157));
#26776=CARTESIAN_POINT('Ctrl Pts',(1.17501305787994,-1.,1.33437539344842));
#26777=CARTESIAN_POINT('Ctrl Pts',(1.17501305787994,1.,1.33437539344842));
#26778=CARTESIAN_POINT('Ctrl Pts',(1.16589330092532,-1.,1.32428080720544));
#26779=CARTESIAN_POINT('Ctrl Pts',(1.16589330092532,1.,1.32428080720544));
#26780=CARTESIAN_POINT('Ctrl Pts',(1.15950888730433,-1.,1.3172297721596));
#26781=CARTESIAN_POINT('Ctrl Pts',(1.15950888730433,1.,1.3172297721596));
#26782=CARTESIAN_POINT('Ctrl Pts',(1.15624053661742,-1.,1.31362392696033));
#26783=CARTESIAN_POINT('Ctrl Pts',(1.15624053661742,1.,1.31362392696033));
#26784=CARTESIAN_POINT('',(1.34869019493419,1.,1.73811241238545));
#26785=CARTESIAN_POINT('Ctrl Pts',(1.34869019493419,1.,1.73811241238545));
#26786=CARTESIAN_POINT('Ctrl Pts',(1.34854391898145,1.,1.73682580585819));
#26787=CARTESIAN_POINT('Ctrl Pts',(1.34824783113158,1.,1.73425417886255));
#26788=CARTESIAN_POINT('Ctrl Pts',(1.3477930915247,1.,1.73040149654497));
#26789=CARTESIAN_POINT('Ctrl Pts',(1.34716554820013,1.,1.72527410681298));
#26790=CARTESIAN_POINT('Ctrl Pts',(1.34634568653586,1.,1.7188807715095));
#26791=CARTESIAN_POINT('Ctrl Pts',(1.34549029589563,1.,1.71250340687011));
#26792=CARTESIAN_POINT('Ctrl Pts',(1.34459924533783,1.,1.70614212266676));
#26793=CARTESIAN_POINT('Ctrl Pts',(1.34367237124322,1.,1.69979707754221));
#26794=CARTESIAN_POINT('Ctrl Pts',(1.34270948206139,1.,1.6934684849664));
#26795=CARTESIAN_POINT('Ctrl Pts',(1.34171037484673,1.,1.68715660868602));
#26796=CARTESIAN_POINT('Ctrl Pts',(1.3406748518516,1.,1.68086176030308));
#26797=CARTESIAN_POINT('Ctrl Pts',(1.33960273470372,1.,1.67458429426126));
#26798=CARTESIAN_POINT('Ctrl Pts',(1.33849388654458,1.,1.66832460784078));
#26799=CARTESIAN_POINT('Ctrl Pts',(1.33734820885331,1.,1.66208312542073));
#26800=CARTESIAN_POINT('Ctrl Pts',(1.33616559745217,1.,1.65586025952651));
#26801=CARTESIAN_POINT('Ctrl Pts',(1.33494590468003,1.,1.64965637286843));
#26802=CARTESIAN_POINT('Ctrl Pts',(1.33368890676554,1.,1.64347174856007));
#26803=CARTESIAN_POINT('Ctrl Pts',(1.33239425103694,1.,1.6373065347505));
#26804=CARTESIAN_POINT('Ctrl Pts',(1.33106149345618,1.,1.63116079730887));
#26805=CARTESIAN_POINT('Ctrl Pts',(1.32969019505665,1.,1.62503464209777));
#26806=CARTESIAN_POINT('Ctrl Pts',(1.32828000610448,1.,1.61892832270723));
#26807=CARTESIAN_POINT('Ctrl Pts',(1.32683074483365,1.,1.61284234015762));
#26808=CARTESIAN_POINT('Ctrl Pts',(1.32534250785794,1.,1.6067775829097));
#26809=CARTESIAN_POINT('Ctrl Pts',(1.32381550858266,1.,1.600735118587));
#26810=CARTESIAN_POINT('Ctrl Pts',(1.32224985747686,1.,1.59471591079408));
#26811=CARTESIAN_POINT('Ctrl Pts',(1.32064537110891,1.,1.58872057258244));
#26812=CARTESIAN_POINT('Ctrl Pts',(1.31900135021428,1.,1.58274907898829));
#26813=CARTESIAN_POINT('Ctrl Pts',(1.31731642317183,1.,1.57680056505585));
#26814=CARTESIAN_POINT('Ctrl Pts',(1.31558903860015,1.,1.57087397835721));
#26815=CARTESIAN_POINT('Ctrl Pts',(1.31381795281002,1.,1.56496872402352));
#26816=CARTESIAN_POINT('Ctrl Pts',(1.31200264341696,1.,1.55908521254822));
#26817=CARTESIAN_POINT('Ctrl Pts',(1.31014393684221,1.,1.55322568759481));
#26818=CARTESIAN_POINT('Ctrl Pts',(1.30824393907471,1.,1.54739413957183));
#26819=CARTESIAN_POINT('Ctrl Pts',(1.30630475189553,1.,1.54159462645428));
#26820=CARTESIAN_POINT('Ctrl Pts',(1.30432735639487,1.,1.53582981268976));
#26821=CARTESIAN_POINT('Ctrl Pts',(1.3023106439557,1.,1.53009970283893));
#26822=CARTESIAN_POINT('Ctrl Pts',(1.30024984366334,1.,1.5243995786107));
#26823=CARTESIAN_POINT('Ctrl Pts',(1.29813791800757,1.,1.51872184912735));
#26824=CARTESIAN_POINT('Ctrl Pts',(1.29596850710518,1.,1.51305994241412));
#26825=CARTESIAN_POINT('Ctrl Pts',(1.29373841372843,1.,1.50741159078367));
#26826=CARTESIAN_POINT('Ctrl Pts',(1.29145022885171,1.,1.50178230149764));
#26827=CARTESIAN_POINT('Ctrl Pts',(1.28911506584232,1.,1.49618896881729));
#26828=CARTESIAN_POINT('Ctrl Pts',(1.28674676116415,1.,1.4906522831275));
#26829=CARTESIAN_POINT('Ctrl Pts',(1.28435533880184,1.,1.48518817118891));
#26830=CARTESIAN_POINT('Ctrl Pts',(1.28194158939522,1.,1.47980070347102));
#26831=CARTESIAN_POINT('Ctrl Pts',(1.27948918248524,1.,1.4744717526711));
#26832=CARTESIAN_POINT('Ctrl Pts',(1.27696414831144,1.,1.46916035917197));
#26833=CARTESIAN_POINT('Ctrl Pts',(1.27433119897877,1.,1.4638243133254));
#26834=CARTESIAN_POINT('Ctrl Pts',(1.27156805265312,1.,1.45843906294725));
#26835=CARTESIAN_POINT('Ctrl Pts',(1.26867786804854,1.,1.45301422764205));
#26836=CARTESIAN_POINT('Ctrl Pts',(1.26570925118767,1.,1.44761985001544));
#26837=CARTESIAN_POINT('Ctrl Pts',(1.26273903323723,1.,1.44236470511145));
#26838=CARTESIAN_POINT('Ctrl Pts',(1.25983531011894,1.,1.43734919180719));
#26839=CARTESIAN_POINT('Ctrl Pts',(1.25702687965744,1.,1.43262645609679));
#26840=CARTESIAN_POINT('Ctrl Pts',(1.25426945222783,1.,1.42815938799555));
#26841=CARTESIAN_POINT('Ctrl Pts',(1.25141455570299,1.,1.42378102115911));
#26842=CARTESIAN_POINT('Ctrl Pts',(1.24824430986911,1.,1.41923722596421));
#26843=CARTESIAN_POINT('Ctrl Pts',(1.24450600513278,1.,1.41422913175437));
#26844=CARTESIAN_POINT('Ctrl Pts',(1.23994455029421,1.,1.40845295531151));
#26845=CARTESIAN_POINT('Ctrl Pts',(1.23434087289768,1.,1.40164708205345));
#26846=CARTESIAN_POINT('Ctrl Pts',(1.22752961898063,1.,1.39361389567257));
#26847=CARTESIAN_POINT('Ctrl Pts',(1.21938737278853,1.,1.38420564525391));
#26848=CARTESIAN_POINT('Ctrl Pts',(1.20982812923113,1.,1.37331915604962));
#26849=CARTESIAN_POINT('Ctrl Pts',(1.1987959077656,1.,1.36088705040677));
#26850=CARTESIAN_POINT('Ctrl Pts',(1.18625865664915,1.,1.34687053998157));
#26851=CARTESIAN_POINT('Ctrl Pts',(1.17501305787994,1.,1.33437539344842));
#26852=CARTESIAN_POINT('Ctrl Pts',(1.16589330092532,1.,1.32428080720544));
#26853=CARTESIAN_POINT('Ctrl Pts',(1.15950888730433,1.,1.3172297721596));
#26854=CARTESIAN_POINT('Ctrl Pts',(1.15624053661742,1.,1.31362392696033));
#26855=CARTESIAN_POINT('',(1.34869019493419,0.,1.73811241238545));
#26856=CARTESIAN_POINT('Origin',(1.23627494547115,0.,1.81978687191668));
#26857=CARTESIAN_POINT('',(1.23627494547115,1.,1.81978687191668));
#26858=CARTESIAN_POINT('',(1.34869019493419,1.,1.73811241238545));
#26859=CARTESIAN_POINT('',(1.23627494547115,0.,1.81978687191668));
#26860=CARTESIAN_POINT('Ctrl Pts',(0.892032620296855,-1.,1.5055822144029));
#26861=CARTESIAN_POINT('Ctrl Pts',(0.892032620296855,1.,1.5055822144029));
#26862=CARTESIAN_POINT('Ctrl Pts',(0.894452006967538,-1.,1.50980486807181));
#26863=CARTESIAN_POINT('Ctrl Pts',(0.894452006967538,1.,1.50980486807181));
#26864=CARTESIAN_POINT('Ctrl Pts',(0.89918504749193,-1.,1.51805569591479));
#26865=CARTESIAN_POINT('Ctrl Pts',(0.89918504749193,1.,1.51805569591479));
#26866=CARTESIAN_POINT('Ctrl Pts',(0.905967409640498,-1.,1.52984849890434));
#26867=CARTESIAN_POINT('Ctrl Pts',(0.905967409640498,1.,1.52984849890434));
#26868=CARTESIAN_POINT('Ctrl Pts',(0.914375919046579,-1.,1.54440491152808));
#26869=CARTESIAN_POINT('Ctrl Pts',(0.914375919046579,1.,1.54440491152808));
#26870=CARTESIAN_POINT('Ctrl Pts',(0.923832188966322,-1.,1.56065988582509));
#26871=CARTESIAN_POINT('Ctrl Pts',(0.923832188966322,1.,1.56065988582509));
#26872=CARTESIAN_POINT('Ctrl Pts',(0.932246680128848,-1.,1.57499388385561));
#26873=CARTESIAN_POINT('Ctrl Pts',(0.932246680128848,1.,1.57499388385561));
#26874=CARTESIAN_POINT('Ctrl Pts',(0.939646377909319,-1.,1.58744937489796));
#26875=CARTESIAN_POINT('Ctrl Pts',(0.939646377909319,1.,1.58744937489796));
#26876=CARTESIAN_POINT('Ctrl Pts',(0.946078063325795,-1.,1.59810042045408));
#26877=CARTESIAN_POINT('Ctrl Pts',(0.946078063325795,1.,1.59810042045408));
#26878=CARTESIAN_POINT('Ctrl Pts',(0.951613284361247,-1.,1.60706069897794));
#26879=CARTESIAN_POINT('Ctrl Pts',(0.951613284361247,1.,1.60706069897794));
#26880=CARTESIAN_POINT('Ctrl Pts',(0.956354422921572,-1.,1.61449324337233));
#26881=CARTESIAN_POINT('Ctrl Pts',(0.956354422921572,1.,1.61449324337233));
#26882=CARTESIAN_POINT('Ctrl Pts',(0.960438326099958,-1.,1.62061638139929));
#26883=CARTESIAN_POINT('Ctrl Pts',(0.960438326099958,1.,1.62061638139929));
#26884=CARTESIAN_POINT('Ctrl Pts',(0.964046107037821,-1.,1.6257193066974));
#26885=CARTESIAN_POINT('Ctrl Pts',(0.964046107037821,1.,1.6257193066974));
#26886=CARTESIAN_POINT('Ctrl Pts',(0.967387853228041,-1.,1.63013849959083));
#26887=CARTESIAN_POINT('Ctrl Pts',(0.967387853228041,1.,1.63013849959083));
#26888=CARTESIAN_POINT('Ctrl Pts',(0.970669715996356,-1.,1.63420665729609));
#26889=CARTESIAN_POINT('Ctrl Pts',(0.970669715996356,1.,1.63420665729609));
#26890=CARTESIAN_POINT('Ctrl Pts',(0.974066058287501,-1.,1.63820952658157));
#26891=CARTESIAN_POINT('Ctrl Pts',(0.974066058287501,1.,1.63820952658157));
#26892=CARTESIAN_POINT('Ctrl Pts',(0.977689794120296,-1.,1.64233990826831));
#26893=CARTESIAN_POINT('Ctrl Pts',(0.977689794120296,1.,1.64233990826831));
#26894=CARTESIAN_POINT('Ctrl Pts',(0.981562530940574,-1.,1.64665139190834));
#26895=CARTESIAN_POINT('Ctrl Pts',(0.981562530940574,1.,1.64665139190834));
#26896=CARTESIAN_POINT('Ctrl Pts',(0.985642622921626,-1.,1.6511001661277));
#26897=CARTESIAN_POINT('Ctrl Pts',(0.985642622921626,1.,1.6511001661277));
#26898=CARTESIAN_POINT('Ctrl Pts',(0.98985562785445,-1.,1.65559044289746));
#26899=CARTESIAN_POINT('Ctrl Pts',(0.98985562785445,1.,1.65559044289746));
#26900=CARTESIAN_POINT('Ctrl Pts',(0.994121836661115,-1.,1.66001553809916));
#26901=CARTESIAN_POINT('Ctrl Pts',(0.994121836661115,1.,1.66001553809916));
#26902=CARTESIAN_POINT('Ctrl Pts',(0.998389654952317,-1.,1.66430758030304));
#26903=CARTESIAN_POINT('Ctrl Pts',(0.998389654952317,1.,1.66430758030304));
#26904=CARTESIAN_POINT('Ctrl Pts',(1.00265091003682,-1.,1.66846059277231));
#26905=CARTESIAN_POINT('Ctrl Pts',(1.00265091003682,1.,1.66846059277231));
#26906=CARTESIAN_POINT('Ctrl Pts',(1.00692206696387,-1.,1.67250335383248));
#26907=CARTESIAN_POINT('Ctrl Pts',(1.00692206696387,1.,1.67250335383248));
#26908=CARTESIAN_POINT('Ctrl Pts',(1.01123236493507,-1.,1.67648246776457));
#26909=CARTESIAN_POINT('Ctrl Pts',(1.01123236493507,1.,1.67648246776457));
#26910=CARTESIAN_POINT('Ctrl Pts',(1.01561026162786,-1.,1.6804428989482));
#26911=CARTESIAN_POINT('Ctrl Pts',(1.01561026162786,1.,1.6804428989482));
#26912=CARTESIAN_POINT('Ctrl Pts',(1.02006795074222,-1.,1.68440578021739));
#26913=CARTESIAN_POINT('Ctrl Pts',(1.02006795074222,1.,1.68440578021739));
#26914=CARTESIAN_POINT('Ctrl Pts',(1.02460180535272,-1.,1.68836910178475));
#26915=CARTESIAN_POINT('Ctrl Pts',(1.02460180535272,1.,1.68836910178475));
#26916=CARTESIAN_POINT('Ctrl Pts',(1.02919977579155,-1.,1.69231840863471));
#26917=CARTESIAN_POINT('Ctrl Pts',(1.02919977579155,1.,1.69231840863471));
#26918=CARTESIAN_POINT('Ctrl Pts',(1.03384646003587,-1.,1.69623414782769));
#26919=CARTESIAN_POINT('Ctrl Pts',(1.03384646003587,1.,1.69623414782769));
#26920=CARTESIAN_POINT('Ctrl Pts',(1.03852922490782,-1.,1.70010052930951));
#26921=CARTESIAN_POINT('Ctrl Pts',(1.03852922490782,1.,1.70010052930951));
#26922=CARTESIAN_POINT('Ctrl Pts',(1.04324363334546,-1.,1.70391338707969));
#26923=CARTESIAN_POINT('Ctrl Pts',(1.04324363334546,1.,1.70391338707969));
#26924=CARTESIAN_POINT('Ctrl Pts',(1.0479908540499,-1.,1.70767646263641));
#26925=CARTESIAN_POINT('Ctrl Pts',(1.0479908540499,1.,1.70767646263641));
#26926=CARTESIAN_POINT('Ctrl Pts',(1.05277517202853,-1.,1.71139783543986));
#26927=CARTESIAN_POINT('Ctrl Pts',(1.05277517202853,1.,1.71139783543986));
#26928=CARTESIAN_POINT('Ctrl Pts',(1.05760163192481,-1.,1.71508654427022));
#26929=CARTESIAN_POINT('Ctrl Pts',(1.05760163192481,1.,1.71508654427022));
#26930=CARTESIAN_POINT('Ctrl Pts',(1.06247324680649,-1.,1.71874858456908));
#26931=CARTESIAN_POINT('Ctrl Pts',(1.06247324680649,1.,1.71874858456908));
#26932=CARTESIAN_POINT('Ctrl Pts',(1.06738966975463,-1.,1.72238500928456));
#26933=CARTESIAN_POINT('Ctrl Pts',(1.06738966975463,1.,1.72238500928456));
#26934=CARTESIAN_POINT('Ctrl Pts',(1.07234866990252,-1.,1.72599406198489));
#26935=CARTESIAN_POINT('Ctrl Pts',(1.07234866990252,1.,1.72599406198489));
#26936=CARTESIAN_POINT('Ctrl Pts',(1.0773470373727,-1.,1.72957248977424));
#26937=CARTESIAN_POINT('Ctrl Pts',(1.0773470373727,1.,1.72957248977424));
#26938=CARTESIAN_POINT('Ctrl Pts',(1.08238162784749,-1.,1.73311705663407));
#26939=CARTESIAN_POINT('Ctrl Pts',(1.08238162784749,1.,1.73311705663407));
#26940=CARTESIAN_POINT('Ctrl Pts',(1.08745056285429,-1.,1.73662628326093));
#26941=CARTESIAN_POINT('Ctrl Pts',(1.08745056285429,1.,1.73662628326093));
#26942=CARTESIAN_POINT('Ctrl Pts',(1.09255329056496,-1.,1.74010053962252));
#26943=CARTESIAN_POINT('Ctrl Pts',(1.09255329056496,1.,1.74010053962252));
#26944=CARTESIAN_POINT('Ctrl Pts',(1.09768999241229,-1.,1.74354119236212));
#26945=CARTESIAN_POINT('Ctrl Pts',(1.09768999241229,1.,1.74354119236212));
#26946=CARTESIAN_POINT('Ctrl Pts',(1.10286118991144,-1.,1.74695004214924));
#26947=CARTESIAN_POINT('Ctrl Pts',(1.10286118991144,1.,1.74695004214924));
#26948=CARTESIAN_POINT('Ctrl Pts',(1.10806728183003,-1.,1.75032866075914));
#26949=CARTESIAN_POINT('Ctrl Pts',(1.10806728183003,1.,1.75032866075914));
#26950=CARTESIAN_POINT('Ctrl Pts',(1.11330807582542,-1.,1.75367772094617));
#26951=CARTESIAN_POINT('Ctrl Pts',(1.11330807582542,1.,1.75367772094617));
#26952=CARTESIAN_POINT('Ctrl Pts',(1.11858293216752,-1.,1.75699720772089));
#26953=CARTESIAN_POINT('Ctrl Pts',(1.11858293216752,1.,1.75699720772089));
#26954=CARTESIAN_POINT('Ctrl Pts',(1.12389096855078,-1.,1.76028671825084));
#26955=CARTESIAN_POINT('Ctrl Pts',(1.12389096855078,1.,1.76028671825084));
#26956=CARTESIAN_POINT('Ctrl Pts',(1.12923123555076,-1.,1.76354571966171));
#26957=CARTESIAN_POINT('Ctrl Pts',(1.12923123555076,1.,1.76354571966171));
#26958=CARTESIAN_POINT('Ctrl Pts',(1.13460291804634,-1.,1.76677384551883));
#26959=CARTESIAN_POINT('Ctrl Pts',(1.13460291804634,1.,1.76677384551883));
#26960=CARTESIAN_POINT('Ctrl Pts',(1.14000548337,-1.,1.76997111386806));
#26961=CARTESIAN_POINT('Ctrl Pts',(1.14000548337,1.,1.76997111386806));
#26962=CARTESIAN_POINT('Ctrl Pts',(1.14543858226948,-1.,1.77313777896234));
#26963=CARTESIAN_POINT('Ctrl Pts',(1.14543858226948,1.,1.77313777896234));
#26964=CARTESIAN_POINT('Ctrl Pts',(1.15090197841531,-1.,1.77627422557034));
#26965=CARTESIAN_POINT('Ctrl Pts',(1.15090197841531,1.,1.77627422557034));
#26966=CARTESIAN_POINT('Ctrl Pts',(1.15639547194689,-1.,1.77938085564261));
#26967=CARTESIAN_POINT('Ctrl Pts',(1.15639547194689,1.,1.77938085564261));
#26968=CARTESIAN_POINT('Ctrl Pts',(1.16191881298458,-1.,1.78245795880949));
#26969=CARTESIAN_POINT('Ctrl Pts',(1.16191881298458,1.,1.78245795880949));
#26970=CARTESIAN_POINT('Ctrl Pts',(1.16747166312239,-1.,1.78550566040349));
#26971=CARTESIAN_POINT('Ctrl Pts',(1.16747166312239,1.,1.78550566040349));
#26972=CARTESIAN_POINT('Ctrl Pts',(1.17305363177265,-1.,1.78852398877523));
#26973=CARTESIAN_POINT('Ctrl Pts',(1.17305363177265,1.,1.78852398877523));
#26974=CARTESIAN_POINT('Ctrl Pts',(1.17866429440781,-1.,1.79151291552646));
#26975=CARTESIAN_POINT('Ctrl Pts',(1.17866429440781,1.,1.79151291552646));
#26976=CARTESIAN_POINT('Ctrl Pts',(1.18430321697471,-1.,1.79447240321572));
#26977=CARTESIAN_POINT('Ctrl Pts',(1.18430321697471,1.,1.79447240321572));
#26978=CARTESIAN_POINT('Ctrl Pts',(1.1899699793456,-1.,1.79740245923649));
#26979=CARTESIAN_POINT('Ctrl Pts',(1.1899699793456,1.,1.79740245923649));
#26980=CARTESIAN_POINT('Ctrl Pts',(1.19566418930405,-1.,1.80030314370121));
#26981=CARTESIAN_POINT('Ctrl Pts',(1.19566418930405,1.,1.80030314370121));
#26982=CARTESIAN_POINT('Ctrl Pts',(1.2013854893912,-1.,1.8031745483882));
#26983=CARTESIAN_POINT('Ctrl Pts',(1.2013854893912,1.,1.8031745483882));
#26984=CARTESIAN_POINT('Ctrl Pts',(1.20713356605519,-1.,1.80601678480772));
#26985=CARTESIAN_POINT('Ctrl Pts',(1.20713356605519,1.,1.80601678480772));
#26986=CARTESIAN_POINT('Ctrl Pts',(1.2129081570818,-1.,1.80882996916931));
#26987=CARTESIAN_POINT('Ctrl Pts',(1.2129081570818,1.,1.80882996916931));
#26988=CARTESIAN_POINT('Ctrl Pts',(1.2187090610323,-1.,1.81161420806172));
#26989=CARTESIAN_POINT('Ctrl Pts',(1.2187090610323,1.,1.81161420806172));
#26990=CARTESIAN_POINT('Ctrl Pts',(1.22453613304507,-1.,1.81436959209778));
#26991=CARTESIAN_POINT('Ctrl Pts',(1.22453613304507,1.,1.81436959209778));
#26992=CARTESIAN_POINT('Ctrl Pts',(1.22921864890975,-1.,1.81655087183054));
#26993=CARTESIAN_POINT('Ctrl Pts',(1.22921864890975,1.,1.81655087183054));
#26994=CARTESIAN_POINT('Ctrl Pts',(1.23274224526804,-1.,1.81817389920914));
#26995=CARTESIAN_POINT('Ctrl Pts',(1.23274224526804,1.,1.81817389920914));
#26996=CARTESIAN_POINT('Ctrl Pts',(1.23509651170384,-1.,1.81925017193531));
#26997=CARTESIAN_POINT('Ctrl Pts',(1.23509651170384,1.,1.81925017193531));
#26998=CARTESIAN_POINT('Ctrl Pts',(1.23627494547115,-1.,1.81978687191668));
#26999=CARTESIAN_POINT('Ctrl Pts',(1.23627494547115,1.,1.81978687191668));
#27000=CARTESIAN_POINT('',(0.892032620296855,1.,1.5055822144029));
#27001=CARTESIAN_POINT('Ctrl Pts',(0.892032620296855,1.,1.5055822144029));
#27002=CARTESIAN_POINT('Ctrl Pts',(0.894452006967538,1.,1.50980486807181));
#27003=CARTESIAN_POINT('Ctrl Pts',(0.89918504749193,1.,1.51805569591479));
#27004=CARTESIAN_POINT('Ctrl Pts',(0.905967409640498,1.,1.52984849890434));
#27005=CARTESIAN_POINT('Ctrl Pts',(0.914375919046579,1.,1.54440491152808));
#27006=CARTESIAN_POINT('Ctrl Pts',(0.923832188966322,1.,1.56065988582509));
#27007=CARTESIAN_POINT('Ctrl Pts',(0.932246680128848,1.,1.57499388385561));
#27008=CARTESIAN_POINT('Ctrl Pts',(0.939646377909319,1.,1.58744937489796));
#27009=CARTESIAN_POINT('Ctrl Pts',(0.946078063325795,1.,1.59810042045408));
#27010=CARTESIAN_POINT('Ctrl Pts',(0.951613284361247,1.,1.60706069897794));
#27011=CARTESIAN_POINT('Ctrl Pts',(0.956354422921572,1.,1.61449324337233));
#27012=CARTESIAN_POINT('Ctrl Pts',(0.960438326099958,1.,1.62061638139929));
#27013=CARTESIAN_POINT('Ctrl Pts',(0.964046107037821,1.,1.6257193066974));
#27014=CARTESIAN_POINT('Ctrl Pts',(0.967387853228041,1.,1.63013849959083));
#27015=CARTESIAN_POINT('Ctrl Pts',(0.970669715996356,1.,1.63420665729609));
#27016=CARTESIAN_POINT('Ctrl Pts',(0.974066058287501,1.,1.63820952658157));
#27017=CARTESIAN_POINT('Ctrl Pts',(0.977689794120296,1.,1.64233990826831));
#27018=CARTESIAN_POINT('Ctrl Pts',(0.981562530940574,1.,1.64665139190834));
#27019=CARTESIAN_POINT('Ctrl Pts',(0.985642622921626,1.,1.6511001661277));
#27020=CARTESIAN_POINT('Ctrl Pts',(0.98985562785445,1.,1.65559044289746));
#27021=CARTESIAN_POINT('Ctrl Pts',(0.994121836661115,1.,1.66001553809916));
#27022=CARTESIAN_POINT('Ctrl Pts',(0.998389654952317,1.,1.66430758030304));
#27023=CARTESIAN_POINT('Ctrl Pts',(1.00265091003682,1.,1.66846059277231));
#27024=CARTESIAN_POINT('Ctrl Pts',(1.00692206696387,1.,1.67250335383248));
#27025=CARTESIAN_POINT('Ctrl Pts',(1.01123236493507,1.,1.67648246776457));
#27026=CARTESIAN_POINT('Ctrl Pts',(1.01561026162786,1.,1.6804428989482));
#27027=CARTESIAN_POINT('Ctrl Pts',(1.02006795074222,1.,1.68440578021739));
#27028=CARTESIAN_POINT('Ctrl Pts',(1.02460180535272,1.,1.68836910178475));
#27029=CARTESIAN_POINT('Ctrl Pts',(1.02919977579155,1.,1.69231840863471));
#27030=CARTESIAN_POINT('Ctrl Pts',(1.03384646003587,1.,1.69623414782769));
#27031=CARTESIAN_POINT('Ctrl Pts',(1.03852922490782,1.,1.70010052930951));
#27032=CARTESIAN_POINT('Ctrl Pts',(1.04324363334546,1.,1.70391338707969));
#27033=CARTESIAN_POINT('Ctrl Pts',(1.0479908540499,1.,1.70767646263641));
#27034=CARTESIAN_POINT('Ctrl Pts',(1.05277517202853,1.,1.71139783543986));
#27035=CARTESIAN_POINT('Ctrl Pts',(1.05760163192481,1.,1.71508654427022));
#27036=CARTESIAN_POINT('Ctrl Pts',(1.06247324680649,1.,1.71874858456908));
#27037=CARTESIAN_POINT('Ctrl Pts',(1.06738966975463,1.,1.72238500928456));
#27038=CARTESIAN_POINT('Ctrl Pts',(1.07234866990252,1.,1.72599406198489));
#27039=CARTESIAN_POINT('Ctrl Pts',(1.0773470373727,1.,1.72957248977424));
#27040=CARTESIAN_POINT('Ctrl Pts',(1.08238162784749,1.,1.73311705663407));
#27041=CARTESIAN_POINT('Ctrl Pts',(1.08745056285429,1.,1.73662628326093));
#27042=CARTESIAN_POINT('Ctrl Pts',(1.09255329056496,1.,1.74010053962252));
#27043=CARTESIAN_POINT('Ctrl Pts',(1.09768999241229,1.,1.74354119236212));
#27044=CARTESIAN_POINT('Ctrl Pts',(1.10286118991144,1.,1.74695004214924));
#27045=CARTESIAN_POINT('Ctrl Pts',(1.10806728183003,1.,1.75032866075914));
#27046=CARTESIAN_POINT('Ctrl Pts',(1.11330807582542,1.,1.75367772094617));
#27047=CARTESIAN_POINT('Ctrl Pts',(1.11858293216752,1.,1.75699720772089));
#27048=CARTESIAN_POINT('Ctrl Pts',(1.12389096855078,1.,1.76028671825084));
#27049=CARTESIAN_POINT('Ctrl Pts',(1.12923123555076,1.,1.76354571966171));
#27050=CARTESIAN_POINT('Ctrl Pts',(1.13460291804634,1.,1.76677384551883));
#27051=CARTESIAN_POINT('Ctrl Pts',(1.14000548337,1.,1.76997111386806));
#27052=CARTESIAN_POINT('Ctrl Pts',(1.14543858226948,1.,1.77313777896234));
#27053=CARTESIAN_POINT('Ctrl Pts',(1.15090197841531,1.,1.77627422557034));
#27054=CARTESIAN_POINT('Ctrl Pts',(1.15639547194689,1.,1.77938085564261));
#27055=CARTESIAN_POINT('Ctrl Pts',(1.16191881298458,1.,1.78245795880949));
#27056=CARTESIAN_POINT('Ctrl Pts',(1.16747166312239,1.,1.78550566040349));
#27057=CARTESIAN_POINT('Ctrl Pts',(1.17305363177265,1.,1.78852398877523));
#27058=CARTESIAN_POINT('Ctrl Pts',(1.17866429440781,1.,1.79151291552646));
#27059=CARTESIAN_POINT('Ctrl Pts',(1.18430321697471,1.,1.79447240321572));
#27060=CARTESIAN_POINT('Ctrl Pts',(1.1899699793456,1.,1.79740245923649));
#27061=CARTESIAN_POINT('Ctrl Pts',(1.19566418930405,1.,1.80030314370121));
#27062=CARTESIAN_POINT('Ctrl Pts',(1.2013854893912,1.,1.8031745483882));
#27063=CARTESIAN_POINT('Ctrl Pts',(1.20713356605519,1.,1.80601678480772));
#27064=CARTESIAN_POINT('Ctrl Pts',(1.2129081570818,1.,1.80882996916931));
#27065=CARTESIAN_POINT('Ctrl Pts',(1.2187090610323,1.,1.81161420806172));
#27066=CARTESIAN_POINT('Ctrl Pts',(1.22453613304507,1.,1.81436959209778));
#27067=CARTESIAN_POINT('Ctrl Pts',(1.22921864890975,1.,1.81655087183054));
#27068=CARTESIAN_POINT('Ctrl Pts',(1.23274224526804,1.,1.81817389920914));
#27069=CARTESIAN_POINT('Ctrl Pts',(1.23509651170384,1.,1.81925017193531));
#27070=CARTESIAN_POINT('Ctrl Pts',(1.23627494547115,1.,1.81978687191668));
#27071=CARTESIAN_POINT('',(0.892032620296854,0.,1.5055822144029));
#27072=CARTESIAN_POINT('Origin',(0.,0.,0.));
#27073=CARTESIAN_POINT('',(0.693717979106305,1.,1.60662857109684));
#27074=CARTESIAN_POINT('Origin',(0.,1.,0.));
#27075=CARTESIAN_POINT('',(0.693717979106305,0.,1.60662857109684));
#27076=CARTESIAN_POINT('Ctrl Pts',(0.7455743247944,-1.,2.0698113262342));
#27077=CARTESIAN_POINT('Ctrl Pts',(0.7455743247944,1.,2.0698113262342));
#27078=CARTESIAN_POINT('Ctrl Pts',(0.745832791378367,-1.,2.06854248895728));
#27079=CARTESIAN_POINT('Ctrl Pts',(0.745832791378367,1.,2.06854248895728));
#27080=CARTESIAN_POINT('Ctrl Pts',(0.7463458715442,-1.,2.06600523016815));
#27081=CARTESIAN_POINT('Ctrl Pts',(0.7463458715442,1.,2.06600523016815));
#27082=CARTESIAN_POINT('Ctrl Pts',(0.747103932787919,-1.,2.06220058927826));
#27083=CARTESIAN_POINT('Ctrl Pts',(0.747103932787919,1.,2.06220058927826));
#27084=CARTESIAN_POINT('Ctrl Pts',(0.748091554183802,-1.,2.05713023031007));
#27085=CARTESIAN_POINT('Ctrl Pts',(0.748091554183802,1.,2.05713023031007));
#27086=CARTESIAN_POINT('Ctrl Pts',(0.749287468665046,-1.,2.05079645592154));
#27087=CARTESIAN_POINT('Ctrl Pts',(0.749287468665046,1.,2.05079645592154));
#27088=CARTESIAN_POINT('Ctrl Pts',(0.750444657875575,-1.,2.04446689147979));
#27089=CARTESIAN_POINT('Ctrl Pts',(0.750444657875575,1.,2.04446689147979));
#27090=CARTESIAN_POINT('Ctrl Pts',(0.751562963361115,-1.,2.03814160092099));
#27091=CARTESIAN_POINT('Ctrl Pts',(0.751562963361115,1.,2.03814160092099));
#27092=CARTESIAN_POINT('Ctrl Pts',(0.75264218048721,-1.,2.03182068456221));
#27093=CARTESIAN_POINT('Ctrl Pts',(0.75264218048721,1.,2.03182068456221));
#27094=CARTESIAN_POINT('Ctrl Pts',(0.753682061112768,-1.,2.02550428623313));
#27095=CARTESIAN_POINT('Ctrl Pts',(0.753682061112768,1.,2.02550428623313));
#27096=CARTESIAN_POINT('Ctrl Pts',(0.754682330722816,-1.,2.01919259405809));
#27097=CARTESIAN_POINT('Ctrl Pts',(0.754682330722816,1.,2.01919259405809));
#27098=CARTESIAN_POINT('Ctrl Pts',(0.755642704957865,-1.,2.01288584328084));
#27099=CARTESIAN_POINT('Ctrl Pts',(0.755642704957865,1.,2.01288584328084));
#27100=CARTESIAN_POINT('Ctrl Pts',(0.75656290464667,-1.,2.0065843158773));
#27101=CARTESIAN_POINT('Ctrl Pts',(0.75656290464667,1.,2.0065843158773));
#27102=CARTESIAN_POINT('Ctrl Pts',(0.757442676862724,-1.,2.00028834739178));
#27103=CARTESIAN_POINT('Ctrl Pts',(0.757442676862724,1.,2.00028834739178));
#27104=CARTESIAN_POINT('Ctrl Pts',(0.758281796766761,-1.,1.99399831098817));
#27105=CARTESIAN_POINT('Ctrl Pts',(0.758281796766761,1.,1.99399831098817));
#27106=CARTESIAN_POINT('Ctrl Pts',(0.759080037802488,-1.,1.98771456680874));
#27107=CARTESIAN_POINT('Ctrl Pts',(0.759080037802488,1.,1.98771456680874));
#27108=CARTESIAN_POINT('Ctrl Pts',(0.75983714745219,-1.,1.98143741418172));
#27109=CARTESIAN_POINT('Ctrl Pts',(0.75983714745219,1.,1.98143741418172));
#27110=CARTESIAN_POINT('Ctrl Pts',(0.760552825409757,-1.,1.97516705321494));
#27111=CARTESIAN_POINT('Ctrl Pts',(0.760552825409757,1.,1.97516705321494));
#27112=CARTESIAN_POINT('Ctrl Pts',(0.76122669048382,-1.,1.96890351582499));
#27113=CARTESIAN_POINT('Ctrl Pts',(0.76122669048382,1.,1.96890351582499));
#27114=CARTESIAN_POINT('Ctrl Pts',(0.761858300014423,-1.,1.96264672744186));
#27115=CARTESIAN_POINT('Ctrl Pts',(0.761858300014423,1.,1.96264672744186));
#27116=CARTESIAN_POINT('Ctrl Pts',(0.762447203806178,-1.,1.95639665309869));
#27117=CARTESIAN_POINT('Ctrl Pts',(0.762447203806178,1.,1.95639665309869));
#27118=CARTESIAN_POINT('Ctrl Pts',(0.762992990878769,-1.,1.95015342590024));
#27119=CARTESIAN_POINT('Ctrl Pts',(0.762992990878769,1.,1.95015342590024));
#27120=CARTESIAN_POINT('Ctrl Pts',(0.763495333538629,-1.,1.9439174661764));
#27121=CARTESIAN_POINT('Ctrl Pts',(0.763495333538629,1.,1.9439174661764));
#27122=CARTESIAN_POINT('Ctrl Pts',(0.763954049121458,-1.,1.93768964875886));
#27123=CARTESIAN_POINT('Ctrl Pts',(0.763954049121458,1.,1.93768964875886));
#27124=CARTESIAN_POINT('Ctrl Pts',(0.76436901067394,-1.,1.93147105496382));
#27125=CARTESIAN_POINT('Ctrl Pts',(0.76436901067394,1.,1.93147105496382));
#27126=CARTESIAN_POINT('Ctrl Pts',(0.764740025488211,-1.,1.92526263537048));
#27127=CARTESIAN_POINT('Ctrl Pts',(0.764740025488211,1.,1.92526263537048));
#27128=CARTESIAN_POINT('Ctrl Pts',(0.765066729667088,-1.,1.91906491634196));
#27129=CARTESIAN_POINT('Ctrl Pts',(0.765066729667088,1.,1.91906491634196));
#27130=CARTESIAN_POINT('Ctrl Pts',(0.765348465884722,-1.,1.91287765805169));
#27131=CARTESIAN_POINT('Ctrl Pts',(0.765348465884722,1.,1.91287765805169));
#27132=CARTESIAN_POINT('Ctrl Pts',(0.765584196937919,-1.,1.90669961402356));
#27133=CARTESIAN_POINT('Ctrl Pts',(0.765584196937919,1.,1.90669961402356));
#27134=CARTESIAN_POINT('Ctrl Pts',(0.765772772593386,-1.,1.90052930393596));
#27135=CARTESIAN_POINT('Ctrl Pts',(0.765772772593386,1.,1.90052930393596));
#27136=CARTESIAN_POINT('Ctrl Pts',(0.765913193856978,-1.,1.89436577771388));
#27137=CARTESIAN_POINT('Ctrl Pts',(0.765913193856978,1.,1.89436577771388));
#27138=CARTESIAN_POINT('Ctrl Pts',(0.766004837062091,-1.,1.88820926433409));
#27139=CARTESIAN_POINT('Ctrl Pts',(0.766004837062091,1.,1.88820926433409));
#27140=CARTESIAN_POINT('Ctrl Pts',(0.766047794851864,-1.,1.88206215302561));
#27141=CARTESIAN_POINT('Ctrl Pts',(0.766047794851864,1.,1.88206215302561));
#27142=CARTESIAN_POINT('Ctrl Pts',(0.766042837036744,-1.,1.87592888967883));
#27143=CARTESIAN_POINT('Ctrl Pts',(0.766042837036744,1.,1.87592888967883));
#27144=CARTESIAN_POINT('Ctrl Pts',(0.765990708546091,-1.,1.86981398314341));
#27145=CARTESIAN_POINT('Ctrl Pts',(0.765990708546091,1.,1.86981398314341));
#27146=CARTESIAN_POINT('Ctrl Pts',(0.765891519092547,-1.,1.86372027063312));
#27147=CARTESIAN_POINT('Ctrl Pts',(0.765891519092547,1.,1.86372027063312));
#27148=CARTESIAN_POINT('Ctrl Pts',(0.765744212909318,-1.,1.85764741390394));
#27149=CARTESIAN_POINT('Ctrl Pts',(0.765744212909318,1.,1.85764741390394));
#27150=CARTESIAN_POINT('Ctrl Pts',(0.765545710619062,-1.,1.85158945130063));
#27151=CARTESIAN_POINT('Ctrl Pts',(0.765545710619062,1.,1.85158945130063));
#27152=CARTESIAN_POINT('Ctrl Pts',(0.765291664862029,-1.,1.84553698875924));
#27153=CARTESIAN_POINT('Ctrl Pts',(0.765291664862029,1.,1.84553698875924));
#27154=CARTESIAN_POINT('Ctrl Pts',(0.764978057881737,-1.,1.83948181064835));
#27155=CARTESIAN_POINT('Ctrl Pts',(0.764978057881737,1.,1.83948181064835));
#27156=CARTESIAN_POINT('Ctrl Pts',(0.764602549687853,-1.,1.83342077227142));
#27157=CARTESIAN_POINT('Ctrl Pts',(0.764602549687853,1.,1.83342077227142));
#27158=CARTESIAN_POINT('Ctrl Pts',(0.764165902605995,-1.,1.82735991200065));
#27159=CARTESIAN_POINT('Ctrl Pts',(0.764165902605995,1.,1.82735991200065));
#27160=CARTESIAN_POINT('Ctrl Pts',(0.763673465462726,-1.,1.82131873145266));
#27161=CARTESIAN_POINT('Ctrl Pts',(0.763673465462726,1.,1.82131873145266));
#27162=CARTESIAN_POINT('Ctrl Pts',(0.763132003836634,-1.,1.8153211840553));
#27163=CARTESIAN_POINT('Ctrl Pts',(0.763132003836634,1.,1.8153211840553));
#27164=CARTESIAN_POINT('Ctrl Pts',(0.762546129463938,-1.,1.80938551463965));
#27165=CARTESIAN_POINT('Ctrl Pts',(0.762546129463938,1.,1.80938551463965));
#27166=CARTESIAN_POINT('Ctrl Pts',(0.761915336443547,-1.,1.80351583877342));
#27167=CARTESIAN_POINT('Ctrl Pts',(0.761915336443547,1.,1.80351583877342));
#27168=CARTESIAN_POINT('Ctrl Pts',(0.761229695230558,-1.,1.79768986997783));
#27169=CARTESIAN_POINT('Ctrl Pts',(0.761229695230558,1.,1.79768986997783));
#27170=CARTESIAN_POINT('Ctrl Pts',(0.760469555880749,-1.,1.7918581561088));
#27171=CARTESIAN_POINT('Ctrl Pts',(0.760469555880749,1.,1.7918581561088));
#27172=CARTESIAN_POINT('Ctrl Pts',(0.759614401110189,-1.,1.78596964884604));
#27173=CARTESIAN_POINT('Ctrl Pts',(0.759614401110189,1.,1.78596964884604));
#27174=CARTESIAN_POINT('Ctrl Pts',(0.758650626677518,-1.,1.77999411220945));
#27175=CARTESIAN_POINT('Ctrl Pts',(0.758650626677518,1.,1.77999411220945));
#27176=CARTESIAN_POINT('Ctrl Pts',(0.757578264077028,-1.,1.77394167108292));
#27177=CARTESIAN_POINT('Ctrl Pts',(0.757578264077028,1.,1.77394167108292));
#27178=CARTESIAN_POINT('Ctrl Pts',(0.75642189602781,-1.,1.76789396002998));
#27179=CARTESIAN_POINT('Ctrl Pts',(0.75642189602781,1.,1.76789396002998));
#27180=CARTESIAN_POINT('Ctrl Pts',(0.755220979974461,-1.,1.76197817240128));
#27181=CARTESIAN_POINT('Ctrl Pts',(0.755220979974461,1.,1.76197817240128));
#27182=CARTESIAN_POINT('Ctrl Pts',(0.754009254027828,-1.,1.75631083600019));
#27183=CARTESIAN_POINT('Ctrl Pts',(0.754009254027828,1.,1.75631083600019));
#27184=CARTESIAN_POINT('Ctrl Pts',(0.752797683531314,-1.,1.75095139468794));
#27185=CARTESIAN_POINT('Ctrl Pts',(0.752797683531314,1.,1.75095139468794));
#27186=CARTESIAN_POINT('Ctrl Pts',(0.751555614164482,-1.,1.74585086852502));
#27187=CARTESIAN_POINT('Ctrl Pts',(0.751555614164482,1.,1.74585086852502));
#27188=CARTESIAN_POINT('Ctrl Pts',(0.750193435981249,-1.,1.74080458267114));
#27189=CARTESIAN_POINT('Ctrl Pts',(0.750193435981249,1.,1.74080458267114));
#27190=CARTESIAN_POINT('Ctrl Pts',(0.74858246295687,-1.,1.7355035168033));
#27191=CARTESIAN_POINT('Ctrl Pts',(0.74858246295687,1.,1.7355035168033));
#27192=CARTESIAN_POINT('Ctrl Pts',(0.746574710097752,-1.,1.72958533647714));
#27193=CARTESIAN_POINT('Ctrl Pts',(0.746574710097752,1.,1.72958533647714));
#27194=CARTESIAN_POINT('Ctrl Pts',(0.744021445433093,-1.,1.72268229916769));
#27195=CARTESIAN_POINT('Ctrl Pts',(0.744021445433093,1.,1.72268229916769));
#27196=CARTESIAN_POINT('Ctrl Pts',(0.74079516202821,-1.,1.71447789751001));
#27197=CARTESIAN_POINT('Ctrl Pts',(0.74079516202821,1.,1.71447789751001));
#27198=CARTESIAN_POINT('Ctrl Pts',(0.736799665716932,-1.,1.70473309004249));
#27199=CARTESIAN_POINT('Ctrl Pts',(0.736799665716932,1.,1.70473309004249));
#27200=CARTESIAN_POINT('Ctrl Pts',(0.731963238685357,-1.,1.69326921972915));
#27201=CARTESIAN_POINT('Ctrl Pts',(0.731963238685357,1.,1.69326921972915));
#27202=CARTESIAN_POINT('Ctrl Pts',(0.726235967982445,-1.,1.67996158451922));
#27203=CARTESIAN_POINT('Ctrl Pts',(0.726235967982445,1.,1.67996158451922));
#27204=CARTESIAN_POINT('Ctrl Pts',(0.719585433787949,-1.,1.66472880551777));
#27205=CARTESIAN_POINT('Ctrl Pts',(0.719585433787949,1.,1.66472880551777));
#27206=CARTESIAN_POINT('Ctrl Pts',(0.711993139340447,-1.,1.64752408828442));
#27207=CARTESIAN_POINT('Ctrl Pts',(0.711993139340447,1.,1.64752408828442));
#27208=CARTESIAN_POINT('Ctrl Pts',(0.705159151977294,-1.,1.6321654166204));
#27209=CARTESIAN_POINT('Ctrl Pts',(0.705159151977294,1.,1.6321654166204));
#27210=CARTESIAN_POINT('Ctrl Pts',(0.699605146398836,-1.,1.61974673471117));
#27211=CARTESIAN_POINT('Ctrl Pts',(0.699605146398836,1.,1.61974673471117));
#27212=CARTESIAN_POINT('Ctrl Pts',(0.69571209787897,-1.,1.61106790957619));
#27213=CARTESIAN_POINT('Ctrl Pts',(0.69571209787897,1.,1.61106790957619));
#27214=CARTESIAN_POINT('Ctrl Pts',(0.693717979106305,-1.,1.60662857109684));
#27215=CARTESIAN_POINT('Ctrl Pts',(0.693717979106305,1.,1.60662857109684));
#27216=CARTESIAN_POINT('',(0.7455743247944,1.,2.0698113262342));
#27217=CARTESIAN_POINT('Ctrl Pts',(0.7455743247944,1.,2.0698113262342));
#27218=CARTESIAN_POINT('Ctrl Pts',(0.745832791378367,1.,2.06854248895728));
#27219=CARTESIAN_POINT('Ctrl Pts',(0.7463458715442,1.,2.06600523016815));
#27220=CARTESIAN_POINT('Ctrl Pts',(0.747103932787919,1.,2.06220058927826));
#27221=CARTESIAN_POINT('Ctrl Pts',(0.748091554183802,1.,2.05713023031007));
#27222=CARTESIAN_POINT('Ctrl Pts',(0.749287468665046,1.,2.05079645592154));
#27223=CARTESIAN_POINT('Ctrl Pts',(0.750444657875575,1.,2.04446689147979));
#27224=CARTESIAN_POINT('Ctrl Pts',(0.751562963361115,1.,2.03814160092099));
#27225=CARTESIAN_POINT('Ctrl Pts',(0.75264218048721,1.,2.03182068456221));
#27226=CARTESIAN_POINT('Ctrl Pts',(0.753682061112768,1.,2.02550428623313));
#27227=CARTESIAN_POINT('Ctrl Pts',(0.754682330722816,1.,2.01919259405809));
#27228=CARTESIAN_POINT('Ctrl Pts',(0.755642704957865,1.,2.01288584328084));
#27229=CARTESIAN_POINT('Ctrl Pts',(0.75656290464667,1.,2.0065843158773));
#27230=CARTESIAN_POINT('Ctrl Pts',(0.757442676862724,1.,2.00028834739178));
#27231=CARTESIAN_POINT('Ctrl Pts',(0.758281796766761,1.,1.99399831098817));
#27232=CARTESIAN_POINT('Ctrl Pts',(0.759080037802488,1.,1.98771456680874));
#27233=CARTESIAN_POINT('Ctrl Pts',(0.75983714745219,1.,1.98143741418172));
#27234=CARTESIAN_POINT('Ctrl Pts',(0.760552825409757,1.,1.97516705321494));
#27235=CARTESIAN_POINT('Ctrl Pts',(0.76122669048382,1.,1.96890351582499));
#27236=CARTESIAN_POINT('Ctrl Pts',(0.761858300014423,1.,1.96264672744186));
#27237=CARTESIAN_POINT('Ctrl Pts',(0.762447203806178,1.,1.95639665309869));
#27238=CARTESIAN_POINT('Ctrl Pts',(0.762992990878769,1.,1.95015342590024));
#27239=CARTESIAN_POINT('Ctrl Pts',(0.763495333538629,1.,1.9439174661764));
#27240=CARTESIAN_POINT('Ctrl Pts',(0.763954049121458,1.,1.93768964875886));
#27241=CARTESIAN_POINT('Ctrl Pts',(0.76436901067394,1.,1.93147105496382));
#27242=CARTESIAN_POINT('Ctrl Pts',(0.764740025488211,1.,1.92526263537048));
#27243=CARTESIAN_POINT('Ctrl Pts',(0.765066729667088,1.,1.91906491634196));
#27244=CARTESIAN_POINT('Ctrl Pts',(0.765348465884722,1.,1.91287765805169));
#27245=CARTESIAN_POINT('Ctrl Pts',(0.765584196937919,1.,1.90669961402356));
#27246=CARTESIAN_POINT('Ctrl Pts',(0.765772772593386,1.,1.90052930393596));
#27247=CARTESIAN_POINT('Ctrl Pts',(0.765913193856978,1.,1.89436577771388));
#27248=CARTESIAN_POINT('Ctrl Pts',(0.766004837062091,1.,1.88820926433409));
#27249=CARTESIAN_POINT('Ctrl Pts',(0.766047794851864,1.,1.88206215302561));
#27250=CARTESIAN_POINT('Ctrl Pts',(0.766042837036744,1.,1.87592888967883));
#27251=CARTESIAN_POINT('Ctrl Pts',(0.765990708546091,1.,1.86981398314341));
#27252=CARTESIAN_POINT('Ctrl Pts',(0.765891519092547,1.,1.86372027063312));
#27253=CARTESIAN_POINT('Ctrl Pts',(0.765744212909318,1.,1.85764741390394));
#27254=CARTESIAN_POINT('Ctrl Pts',(0.765545710619062,1.,1.85158945130063));
#27255=CARTESIAN_POINT('Ctrl Pts',(0.765291664862029,1.,1.84553698875924));
#27256=CARTESIAN_POINT('Ctrl Pts',(0.764978057881737,1.,1.83948181064835));
#27257=CARTESIAN_POINT('Ctrl Pts',(0.764602549687853,1.,1.83342077227142));
#27258=CARTESIAN_POINT('Ctrl Pts',(0.764165902605995,1.,1.82735991200065));
#27259=CARTESIAN_POINT('Ctrl Pts',(0.763673465462726,1.,1.82131873145266));
#27260=CARTESIAN_POINT('Ctrl Pts',(0.763132003836634,1.,1.8153211840553));
#27261=CARTESIAN_POINT('Ctrl Pts',(0.762546129463938,1.,1.80938551463965));
#27262=CARTESIAN_POINT('Ctrl Pts',(0.761915336443547,1.,1.80351583877342));
#27263=CARTESIAN_POINT('Ctrl Pts',(0.761229695230558,1.,1.79768986997783));
#27264=CARTESIAN_POINT('Ctrl Pts',(0.760469555880749,1.,1.7918581561088));
#27265=CARTESIAN_POINT('Ctrl Pts',(0.759614401110189,1.,1.78596964884604));
#27266=CARTESIAN_POINT('Ctrl Pts',(0.758650626677518,1.,1.77999411220945));
#27267=CARTESIAN_POINT('Ctrl Pts',(0.757578264077028,1.,1.77394167108292));
#27268=CARTESIAN_POINT('Ctrl Pts',(0.75642189602781,1.,1.76789396002998));
#27269=CARTESIAN_POINT('Ctrl Pts',(0.755220979974461,1.,1.76197817240128));
#27270=CARTESIAN_POINT('Ctrl Pts',(0.754009254027828,1.,1.75631083600019));
#27271=CARTESIAN_POINT('Ctrl Pts',(0.752797683531314,1.,1.75095139468794));
#27272=CARTESIAN_POINT('Ctrl Pts',(0.751555614164482,1.,1.74585086852502));
#27273=CARTESIAN_POINT('Ctrl Pts',(0.750193435981249,1.,1.74080458267114));
#27274=CARTESIAN_POINT('Ctrl Pts',(0.74858246295687,1.,1.7355035168033));
#27275=CARTESIAN_POINT('Ctrl Pts',(0.746574710097752,1.,1.72958533647714));
#27276=CARTESIAN_POINT('Ctrl Pts',(0.744021445433093,1.,1.72268229916769));
#27277=CARTESIAN_POINT('Ctrl Pts',(0.74079516202821,1.,1.71447789751001));
#27278=CARTESIAN_POINT('Ctrl Pts',(0.736799665716932,1.,1.70473309004249));
#27279=CARTESIAN_POINT('Ctrl Pts',(0.731963238685357,1.,1.69326921972915));
#27280=CARTESIAN_POINT('Ctrl Pts',(0.726235967982445,1.,1.67996158451922));
#27281=CARTESIAN_POINT('Ctrl Pts',(0.719585433787949,1.,1.66472880551777));
#27282=CARTESIAN_POINT('Ctrl Pts',(0.711993139340447,1.,1.64752408828442));
#27283=CARTESIAN_POINT('Ctrl Pts',(0.705159151977294,1.,1.6321654166204));
#27284=CARTESIAN_POINT('Ctrl Pts',(0.699605146398836,1.,1.61974673471117));
#27285=CARTESIAN_POINT('Ctrl Pts',(0.69571209787897,1.,1.61106790957619));
#27286=CARTESIAN_POINT('Ctrl Pts',(0.693717979106305,1.,1.60662857109684));
#27287=CARTESIAN_POINT('',(0.7455743247944,0.,2.0698113262342));
#27288=CARTESIAN_POINT('Origin',(0.61342227326009,0.,2.11275013067528));
#27289=CARTESIAN_POINT('',(0.61342227326009,1.,2.11275013067528));
#27290=CARTESIAN_POINT('',(0.7455743247944,1.,2.0698113262342));
#27291=CARTESIAN_POINT('',(0.61342227326009,0.,2.11275013067528));
#27292=CARTESIAN_POINT('Ctrl Pts',(0.383122945602004,-1.,1.7075470150345));
#27293=CARTESIAN_POINT('Ctrl Pts',(0.383122945602004,1.,1.7075470150345));
#27294=CARTESIAN_POINT('Ctrl Pts',(0.384119047315541,-1.,1.71231062891958));
#27295=CARTESIAN_POINT('Ctrl Pts',(0.384119047315541,1.,1.71231062891958));
#27296=CARTESIAN_POINT('Ctrl Pts',(0.38607079032701,-1.,1.72162022246158));
#27297=CARTESIAN_POINT('Ctrl Pts',(0.38607079032701,1.,1.72162022246158));
#27298=CARTESIAN_POINT('Ctrl Pts',(0.388877023509191,-1.,1.7349317097561));
#27299=CARTESIAN_POINT('Ctrl Pts',(0.388877023509191,1.,1.7349317097561));
#27300=CARTESIAN_POINT('Ctrl Pts',(0.392375812294307,-1.,1.75137405313962));
#27301=CARTESIAN_POINT('Ctrl Pts',(0.392375812294307,1.,1.75137405313962));
#27302=CARTESIAN_POINT('Ctrl Pts',(0.39634619612042,-1.,1.7697556004756));
#27303=CARTESIAN_POINT('Ctrl Pts',(0.39634619612042,1.,1.7697556004756));
#27304=CARTESIAN_POINT('Ctrl Pts',(0.39991940378308,-1.,1.78598826347533));
#27305=CARTESIAN_POINT('Ctrl Pts',(0.39991940378308,1.,1.78598826347533));
#27306=CARTESIAN_POINT('Ctrl Pts',(0.403107976170441,-1.,1.80012077176221));
#27307=CARTESIAN_POINT('Ctrl Pts',(0.403107976170441,1.,1.80012077176221));
#27308=CARTESIAN_POINT('Ctrl Pts',(0.405933518411838,-1.,1.81223801813988));
#27309=CARTESIAN_POINT('Ctrl Pts',(0.405933518411838,1.,1.81223801813988));
#27310=CARTESIAN_POINT('Ctrl Pts',(0.408428948108533,-1.,1.8224702267854));
#27311=CARTESIAN_POINT('Ctrl Pts',(0.408428948108533,1.,1.8224702267854));
#27312=CARTESIAN_POINT('Ctrl Pts',(0.410641256301674,-1.,1.83100408895216));
#27313=CARTESIAN_POINT('Ctrl Pts',(0.410641256301674,1.,1.83100408895216));
#27314=CARTESIAN_POINT('Ctrl Pts',(0.412633125322161,-1.,1.83808953475839));
#27315=CARTESIAN_POINT('Ctrl Pts',(0.412633125322161,1.,1.83808953475839));
#27316=CARTESIAN_POINT('Ctrl Pts',(0.41448743825434,-1.,1.8440575707371));
#27317=CARTESIAN_POINT('Ctrl Pts',(0.41448743825434,1.,1.8440575707371));
#27318=CARTESIAN_POINT('Ctrl Pts',(0.416300022038864,-1.,1.84929312929882));
#27319=CARTESIAN_POINT('Ctrl Pts',(0.416300022038864,1.,1.84929312929882));
#27320=CARTESIAN_POINT('Ctrl Pts',(0.418164129143534,-1.,1.85417632856234));
#27321=CARTESIAN_POINT('Ctrl Pts',(0.418164129143534,1.,1.85417632856234));
#27322=CARTESIAN_POINT('Ctrl Pts',(0.420157287975619,-1.,1.85903281096686));
#27323=CARTESIAN_POINT('Ctrl Pts',(0.420157287975619,1.,1.85903281096686));
#27324=CARTESIAN_POINT('Ctrl Pts',(0.422327307418275,-1.,1.86408083334028));
#27325=CARTESIAN_POINT('Ctrl Pts',(0.422327307418275,1.,1.86408083334028));
#27326=CARTESIAN_POINT('Ctrl Pts',(0.424678177291358,-1.,1.86937803944323));
#27327=CARTESIAN_POINT('Ctrl Pts',(0.424678177291358,1.,1.86937803944323));
#27328=CARTESIAN_POINT('Ctrl Pts',(0.427183828519102,-1.,1.87486989291484));
#27329=CARTESIAN_POINT('Ctrl Pts',(0.427183828519102,1.,1.87486989291484));
#27330=CARTESIAN_POINT('Ctrl Pts',(0.429803062482344,-1.,1.88044229001832));
#27331=CARTESIAN_POINT('Ctrl Pts',(0.429803062482344,1.,1.88044229001832));
#27332=CARTESIAN_POINT('Ctrl Pts',(0.432493038548748,-1.,1.88596913666793));
#27333=CARTESIAN_POINT('Ctrl Pts',(0.432493038548748,1.,1.88596913666793));
#27334=CARTESIAN_POINT('Ctrl Pts',(0.435225660963383,-1.,1.89136993975504));
#27335=CARTESIAN_POINT('Ctrl Pts',(0.435225660963383,1.,1.89136993975504));
#27336=CARTESIAN_POINT('Ctrl Pts',(0.437995003948244,-1.,1.89663648956466));
#27337=CARTESIAN_POINT('Ctrl Pts',(0.437995003948244,1.,1.89663648956466));
#27338=CARTESIAN_POINT('Ctrl Pts',(0.440807833704038,-1.,1.90180124389086));
#27339=CARTESIAN_POINT('Ctrl Pts',(0.440807833704038,1.,1.90180124389086));
#27340=CARTESIAN_POINT('Ctrl Pts',(0.44367755684915,-1.,1.90691756144898));
#27341=CARTESIAN_POINT('Ctrl Pts',(0.44367755684915,1.,1.90691756144898));
#27342=CARTESIAN_POINT('Ctrl Pts',(0.446617343485711,-1.,1.9120369998112));
#27343=CARTESIAN_POINT('Ctrl Pts',(0.446617343485711,1.,1.9120369998112));
#27344=CARTESIAN_POINT('Ctrl Pts',(0.449632260106662,-1.,1.91718342555755));
#27345=CARTESIAN_POINT('Ctrl Pts',(0.449632260106662,1.,1.91718342555755));
#27346=CARTESIAN_POINT('Ctrl Pts',(0.452719478359432,-1.,1.92235380648502));
#27347=CARTESIAN_POINT('Ctrl Pts',(0.452719478359432,1.,1.92235380648502));
#27348=CARTESIAN_POINT('Ctrl Pts',(0.45587200517437,-1.,1.92753067150476));
#27349=CARTESIAN_POINT('Ctrl Pts',(0.45587200517437,1.,1.92753067150476));
#27350=CARTESIAN_POINT('Ctrl Pts',(0.459081234547926,-1.,1.93269066517934));
#27351=CARTESIAN_POINT('Ctrl Pts',(0.459081234547926,1.,1.93269066517934));
#27352=CARTESIAN_POINT('Ctrl Pts',(0.462340031009056,-1.,1.93781486640821));
#27353=CARTESIAN_POINT('Ctrl Pts',(0.462340031009056,1.,1.93781486640821));
#27354=CARTESIAN_POINT('Ctrl Pts',(0.46564546202603,-1.,1.9428979419619));
#27355=CARTESIAN_POINT('Ctrl Pts',(0.46564546202603,1.,1.9428979419619));
#27356=CARTESIAN_POINT('Ctrl Pts',(0.468997482913135,-1.,1.94794381136514));
#27357=CARTESIAN_POINT('Ctrl Pts',(0.468997482913135,1.,1.94794381136514));
#27358=CARTESIAN_POINT('Ctrl Pts',(0.472397672264072,-1.,1.95296148278133));
#27359=CARTESIAN_POINT('Ctrl Pts',(0.472397672264072,1.,1.95296148278133));
#27360=CARTESIAN_POINT('Ctrl Pts',(0.475848034683176,-1.,1.95796111148177));
#27361=CARTESIAN_POINT('Ctrl Pts',(0.475848034683176,1.,1.95796111148177));
#27362=CARTESIAN_POINT('Ctrl Pts',(0.479349583074855,-1.,1.96294933055943));
#27363=CARTESIAN_POINT('Ctrl Pts',(0.479349583074855,1.,1.96294933055943));
#27364=CARTESIAN_POINT('Ctrl Pts',(0.48290166212069,-1.,1.96792703422362));
#27365=CARTESIAN_POINT('Ctrl Pts',(0.48290166212069,1.,1.96792703422362));
#27366=CARTESIAN_POINT('Ctrl Pts',(0.486502692907658,-1.,1.97289186263272));
#27367=CARTESIAN_POINT('Ctrl Pts',(0.486502692907658,1.,1.97289186263272));
#27368=CARTESIAN_POINT('Ctrl Pts',(0.490150627860952,-1.,1.97783973019229));
#27369=CARTESIAN_POINT('Ctrl Pts',(0.490150627860952,1.,1.97783973019229));
#27370=CARTESIAN_POINT('Ctrl Pts',(0.493843476541494,-1.,1.98276658761821));
#27371=CARTESIAN_POINT('Ctrl Pts',(0.493843476541494,1.,1.98276658761821));
#27372=CARTESIAN_POINT('Ctrl Pts',(0.497579909545574,-1.,1.98767044752932));
#27373=CARTESIAN_POINT('Ctrl Pts',(0.497579909545574,1.,1.98767044752932));
#27374=CARTESIAN_POINT('Ctrl Pts',(0.501359287727146,-1.,1.99255149126155));
#27375=CARTESIAN_POINT('Ctrl Pts',(0.501359287727146,1.,1.99255149126155));
#27376=CARTESIAN_POINT('Ctrl Pts',(0.505181361323026,-1.,1.99741107463572));
#27377=CARTESIAN_POINT('Ctrl Pts',(0.505181361323026,1.,1.99741107463572));
#27378=CARTESIAN_POINT('Ctrl Pts',(0.509046069886157,-1.,2.00225107134734));
#27379=CARTESIAN_POINT('Ctrl Pts',(0.509046069886157,1.,2.00225107134734));
#27380=CARTESIAN_POINT('Ctrl Pts',(0.512953306961792,-1.,2.00707309946949));
#27381=CARTESIAN_POINT('Ctrl Pts',(0.512953306961792,1.,2.00707309946949));
#27382=CARTESIAN_POINT('Ctrl Pts',(0.516902681728687,-1.,2.01187773939242));
#27383=CARTESIAN_POINT('Ctrl Pts',(0.516902681728687,1.,2.01187773939242));
#27384=CARTESIAN_POINT('Ctrl Pts',(0.52089359039937,-1.,2.01666477917286));
#27385=CARTESIAN_POINT('Ctrl Pts',(0.52089359039937,1.,2.01666477917286));
#27386=CARTESIAN_POINT('Ctrl Pts',(0.524925318333476,-1.,2.02143356304698));
#27387=CARTESIAN_POINT('Ctrl Pts',(0.524925318333476,1.,2.02143356304698));
#27388=CARTESIAN_POINT('Ctrl Pts',(0.528997127241914,-1.,2.0261832908329));
#27389=CARTESIAN_POINT('Ctrl Pts',(0.528997127241914,1.,2.0261832908329));
#27390=CARTESIAN_POINT('Ctrl Pts',(0.533108355132976,-1.,2.03091336214426));
#27391=CARTESIAN_POINT('Ctrl Pts',(0.533108355132976,1.,2.03091336214426));
#27392=CARTESIAN_POINT('Ctrl Pts',(0.537258489833262,-1.,2.03562362954037));
#27393=CARTESIAN_POINT('Ctrl Pts',(0.537258489833262,1.,2.03562362954037));
#27394=CARTESIAN_POINT('Ctrl Pts',(0.541447120615659,-1.,2.04031422690527));
#27395=CARTESIAN_POINT('Ctrl Pts',(0.541447120615659,1.,2.04031422690527));
#27396=CARTESIAN_POINT('Ctrl Pts',(0.54567390381743,-1.,2.04498544714588));
#27397=CARTESIAN_POINT('Ctrl Pts',(0.54567390381743,1.,2.04498544714588));
#27398=CARTESIAN_POINT('Ctrl Pts',(0.549938525150295,-1.,2.04963761077958));
#27399=CARTESIAN_POINT('Ctrl Pts',(0.549938525150295,1.,2.04963761077958));
#27400=CARTESIAN_POINT('Ctrl Pts',(0.554240657463906,-1.,2.05427091604413));
#27401=CARTESIAN_POINT('Ctrl Pts',(0.554240657463906,1.,2.05427091604413));
#27402=CARTESIAN_POINT('Ctrl Pts',(0.558579940185151,-1.,2.05888537756462));
#27403=CARTESIAN_POINT('Ctrl Pts',(0.558579940185151,1.,2.05888537756462));
#27404=CARTESIAN_POINT('Ctrl Pts',(0.562955993082261,-1.,2.06348090160589));
#27405=CARTESIAN_POINT('Ctrl Pts',(0.562955993082261,1.,2.06348090160589));
#27406=CARTESIAN_POINT('Ctrl Pts',(0.567368421181087,-1.,2.06805732997334));
#27407=CARTESIAN_POINT('Ctrl Pts',(0.567368421181087,1.,2.06805732997334));
#27408=CARTESIAN_POINT('Ctrl Pts',(0.571816823242602,-1.,2.07261449292824));
#27409=CARTESIAN_POINT('Ctrl Pts',(0.571816823242602,1.,2.07261449292824));
#27410=CARTESIAN_POINT('Ctrl Pts',(0.576300797416844,-1.,2.07715226767559));
#27411=CARTESIAN_POINT('Ctrl Pts',(0.576300797416844,1.,2.07715226767559));
#27412=CARTESIAN_POINT('Ctrl Pts',(0.580819952108063,-1.,2.08167059018418));
#27413=CARTESIAN_POINT('Ctrl Pts',(0.580819952108063,1.,2.08167059018418));
#27414=CARTESIAN_POINT('Ctrl Pts',(0.585373918991617,-1.,2.08616943727951));
#27415=CARTESIAN_POINT('Ctrl Pts',(0.585373918991617,1.,2.08616943727951));
#27416=CARTESIAN_POINT('Ctrl Pts',(0.589962365403406,-1.,2.09064881812129));
#27417=CARTESIAN_POINT('Ctrl Pts',(0.589962365403406,1.,2.09064881812129));
#27418=CARTESIAN_POINT('Ctrl Pts',(0.594585006052162,-1.,2.0951087622027));
#27419=CARTESIAN_POINT('Ctrl Pts',(0.594585006052162,1.,2.0951087622027));
#27420=CARTESIAN_POINT('Ctrl Pts',(0.599241616420533,-1.,2.0995493086477));
#27421=CARTESIAN_POINT('Ctrl Pts',(0.599241616420533,1.,2.0995493086477));
#27422=CARTESIAN_POINT('Ctrl Pts',(0.60393203073603,-1.,2.10397049886949));
#27423=CARTESIAN_POINT('Ctrl Pts',(0.60393203073603,1.,2.10397049886949));
#27424=CARTESIAN_POINT('Ctrl Pts',(0.607711315454876,-1.,2.1074919961518));
#27425=CARTESIAN_POINT('Ctrl Pts',(0.607711315454876,1.,2.1074919961518));
#27426=CARTESIAN_POINT('Ctrl Pts',(0.610560911689898,-1.,2.11012443807238));
#27427=CARTESIAN_POINT('Ctrl Pts',(0.610560911689898,1.,2.11012443807238));
#27428=CARTESIAN_POINT('Ctrl Pts',(0.6124673655618,-1.,2.11187554259986));
#27429=CARTESIAN_POINT('Ctrl Pts',(0.6124673655618,1.,2.11187554259986));
#27430=CARTESIAN_POINT('Ctrl Pts',(0.61342227326009,-1.,2.11275013067528));
#27431=CARTESIAN_POINT('Ctrl Pts',(0.61342227326009,1.,2.11275013067528));
#27432=CARTESIAN_POINT('',(0.383122945602004,1.,1.7075470150345));
#27433=CARTESIAN_POINT('Ctrl Pts',(0.383122945602004,1.,1.7075470150345));
#27434=CARTESIAN_POINT('Ctrl Pts',(0.384119047315541,1.,1.71231062891958));
#27435=CARTESIAN_POINT('Ctrl Pts',(0.38607079032701,1.,1.72162022246158));
#27436=CARTESIAN_POINT('Ctrl Pts',(0.388877023509191,1.,1.7349317097561));
#27437=CARTESIAN_POINT('Ctrl Pts',(0.392375812294307,1.,1.75137405313962));
#27438=CARTESIAN_POINT('Ctrl Pts',(0.39634619612042,1.,1.7697556004756));
#27439=CARTESIAN_POINT('Ctrl Pts',(0.39991940378308,1.,1.78598826347533));
#27440=CARTESIAN_POINT('Ctrl Pts',(0.403107976170441,1.,1.80012077176221));
#27441=CARTESIAN_POINT('Ctrl Pts',(0.405933518411838,1.,1.81223801813988));
#27442=CARTESIAN_POINT('Ctrl Pts',(0.408428948108533,1.,1.8224702267854));
#27443=CARTESIAN_POINT('Ctrl Pts',(0.410641256301674,1.,1.83100408895216));
#27444=CARTESIAN_POINT('Ctrl Pts',(0.412633125322161,1.,1.83808953475839));
#27445=CARTESIAN_POINT('Ctrl Pts',(0.41448743825434,1.,1.8440575707371));
#27446=CARTESIAN_POINT('Ctrl Pts',(0.416300022038864,1.,1.84929312929882));
#27447=CARTESIAN_POINT('Ctrl Pts',(0.418164129143534,1.,1.85417632856234));
#27448=CARTESIAN_POINT('Ctrl Pts',(0.420157287975619,1.,1.85903281096686));
#27449=CARTESIAN_POINT('Ctrl Pts',(0.422327307418275,1.,1.86408083334028));
#27450=CARTESIAN_POINT('Ctrl Pts',(0.424678177291358,1.,1.86937803944323));
#27451=CARTESIAN_POINT('Ctrl Pts',(0.427183828519102,1.,1.87486989291484));
#27452=CARTESIAN_POINT('Ctrl Pts',(0.429803062482344,1.,1.88044229001832));
#27453=CARTESIAN_POINT('Ctrl Pts',(0.432493038548748,1.,1.88596913666793));
#27454=CARTESIAN_POINT('Ctrl Pts',(0.435225660963383,1.,1.89136993975504));
#27455=CARTESIAN_POINT('Ctrl Pts',(0.437995003948244,1.,1.89663648956466));
#27456=CARTESIAN_POINT('Ctrl Pts',(0.440807833704038,1.,1.90180124389086));
#27457=CARTESIAN_POINT('Ctrl Pts',(0.44367755684915,1.,1.90691756144898));
#27458=CARTESIAN_POINT('Ctrl Pts',(0.446617343485711,1.,1.9120369998112));
#27459=CARTESIAN_POINT('Ctrl Pts',(0.449632260106662,1.,1.91718342555755));
#27460=CARTESIAN_POINT('Ctrl Pts',(0.452719478359432,1.,1.92235380648502));
#27461=CARTESIAN_POINT('Ctrl Pts',(0.45587200517437,1.,1.92753067150476));
#27462=CARTESIAN_POINT('Ctrl Pts',(0.459081234547926,1.,1.93269066517934));
#27463=CARTESIAN_POINT('Ctrl Pts',(0.462340031009056,1.,1.93781486640821));
#27464=CARTESIAN_POINT('Ctrl Pts',(0.46564546202603,1.,1.9428979419619));
#27465=CARTESIAN_POINT('Ctrl Pts',(0.468997482913135,1.,1.94794381136514));
#27466=CARTESIAN_POINT('Ctrl Pts',(0.472397672264072,1.,1.95296148278133));
#27467=CARTESIAN_POINT('Ctrl Pts',(0.475848034683176,1.,1.95796111148177));
#27468=CARTESIAN_POINT('Ctrl Pts',(0.479349583074855,1.,1.96294933055943));
#27469=CARTESIAN_POINT('Ctrl Pts',(0.48290166212069,1.,1.96792703422362));
#27470=CARTESIAN_POINT('Ctrl Pts',(0.486502692907658,1.,1.97289186263272));
#27471=CARTESIAN_POINT('Ctrl Pts',(0.490150627860952,1.,1.97783973019229));
#27472=CARTESIAN_POINT('Ctrl Pts',(0.493843476541494,1.,1.98276658761821));
#27473=CARTESIAN_POINT('Ctrl Pts',(0.497579909545574,1.,1.98767044752932));
#27474=CARTESIAN_POINT('Ctrl Pts',(0.501359287727146,1.,1.99255149126155));
#27475=CARTESIAN_POINT('Ctrl Pts',(0.505181361323026,1.,1.99741107463572));
#27476=CARTESIAN_POINT('Ctrl Pts',(0.509046069886157,1.,2.00225107134734));
#27477=CARTESIAN_POINT('Ctrl Pts',(0.512953306961792,1.,2.00707309946949));
#27478=CARTESIAN_POINT('Ctrl Pts',(0.516902681728687,1.,2.01187773939242));
#27479=CARTESIAN_POINT('Ctrl Pts',(0.52089359039937,1.,2.01666477917286));
#27480=CARTESIAN_POINT('Ctrl Pts',(0.524925318333476,1.,2.02143356304698));
#27481=CARTESIAN_POINT('Ctrl Pts',(0.528997127241914,1.,2.0261832908329));
#27482=CARTESIAN_POINT('Ctrl Pts',(0.533108355132976,1.,2.03091336214426));
#27483=CARTESIAN_POINT('Ctrl Pts',(0.537258489833262,1.,2.03562362954037));
#27484=CARTESIAN_POINT('Ctrl Pts',(0.541447120615659,1.,2.04031422690527));
#27485=CARTESIAN_POINT('Ctrl Pts',(0.54567390381743,1.,2.04498544714588));
#27486=CARTESIAN_POINT('Ctrl Pts',(0.549938525150295,1.,2.04963761077958));
#27487=CARTESIAN_POINT('Ctrl Pts',(0.554240657463906,1.,2.05427091604413));
#27488=CARTESIAN_POINT('Ctrl Pts',(0.558579940185151,1.,2.05888537756462));
#27489=CARTESIAN_POINT('Ctrl Pts',(0.562955993082261,1.,2.06348090160589));
#27490=CARTESIAN_POINT('Ctrl Pts',(0.567368421181087,1.,2.06805732997334));
#27491=CARTESIAN_POINT('Ctrl Pts',(0.571816823242602,1.,2.07261449292824));
#27492=CARTESIAN_POINT('Ctrl Pts',(0.576300797416844,1.,2.07715226767559));
#27493=CARTESIAN_POINT('Ctrl Pts',(0.580819952108063,1.,2.08167059018418));
#27494=CARTESIAN_POINT('Ctrl Pts',(0.585373918991617,1.,2.08616943727951));
#27495=CARTESIAN_POINT('Ctrl Pts',(0.589962365403406,1.,2.09064881812129));
#27496=CARTESIAN_POINT('Ctrl Pts',(0.594585006052162,1.,2.0951087622027));
#27497=CARTESIAN_POINT('Ctrl Pts',(0.599241616420533,1.,2.0995493086477));
#27498=CARTESIAN_POINT('Ctrl Pts',(0.60393203073603,1.,2.10397049886949));
#27499=CARTESIAN_POINT('Ctrl Pts',(0.607711315454876,1.,2.1074919961518));
#27500=CARTESIAN_POINT('Ctrl Pts',(0.610560911689898,1.,2.11012443807238));
#27501=CARTESIAN_POINT('Ctrl Pts',(0.6124673655618,1.,2.11187554259986));
#27502=CARTESIAN_POINT('Ctrl Pts',(0.61342227326009,1.,2.11275013067528));
#27503=CARTESIAN_POINT('',(0.383122945602003,0.,1.7075470150345));
#27504=CARTESIAN_POINT('Origin',(0.,0.,0.));
#27505=CARTESIAN_POINT('',(0.163289472382896,1.,1.74236521665491));
#27506=CARTESIAN_POINT('Origin',(0.,1.,0.));
#27507=CARTESIAN_POINT('',(0.163289472382896,0.,1.74236521665491));
#27508=CARTESIAN_POINT('Ctrl Pts',(0.0694764450219578,-1.,2.19890268624765));
#27509=CARTESIAN_POINT('Ctrl Pts',(0.0694764450219578,1.,2.19890268624765));
#27510=CARTESIAN_POINT('Ctrl Pts',(0.0701143536325487,-1.,2.19777582085423));
#27511=CARTESIAN_POINT('Ctrl Pts',(0.0701143536325487,1.,2.19777582085423));
#27512=CARTESIAN_POINT('Ctrl Pts',(0.0713863779526151,-1.,2.19552129484002));
#27513=CARTESIAN_POINT('Ctrl Pts',(0.0713863779526151,1.,2.19552129484002));
#27514=CARTESIAN_POINT('Ctrl Pts',(0.0732830357306722,-1.,2.19213712013662));
#27515=CARTESIAN_POINT('Ctrl Pts',(0.0732830357306722,1.,2.19213712013662));
#27516=CARTESIAN_POINT('Ctrl Pts',(0.0757891465836145,-1.,2.1876201139953));
#27517=CARTESIAN_POINT('Ctrl Pts',(0.0757891465836145,1.,2.1876201139953));
#27518=CARTESIAN_POINT('Ctrl Pts',(0.078883772768524,-1.,2.18196589448887));
#27519=CARTESIAN_POINT('Ctrl Pts',(0.078883772768524,1.,2.18196589448887));
#27520=CARTESIAN_POINT('Ctrl Pts',(0.0819402680872763,-1.,2.176303712113));
#27521=CARTESIAN_POINT('Ctrl Pts',(0.0819402680872763,1.,2.176303712113));
#27522=CARTESIAN_POINT('Ctrl Pts',(0.084958462083537,-1.,2.17063357870952));
#27523=CARTESIAN_POINT('Ctrl Pts',(0.084958462083537,1.,2.17063357870952));
#27524=CARTESIAN_POINT('Ctrl Pts',(0.087938129138692,-1.,2.16495552645014));
#27525=CARTESIAN_POINT('Ctrl Pts',(0.087938129138692,1.,2.16495552645014));
#27526=CARTESIAN_POINT('Ctrl Pts',(0.0908789888107263,-1.,2.15926961544516));
#27527=CARTESIAN_POINT('Ctrl Pts',(0.0908789888107263,1.,2.15926961544516));
#27528=CARTESIAN_POINT('Ctrl Pts',(0.0937807218867641,-1.,2.1535759397817));
#27529=CARTESIAN_POINT('Ctrl Pts',(0.0937807218867641,1.,2.1535759397817));
#27530=CARTESIAN_POINT('Ctrl Pts',(0.0966429852305456,-1.,2.14787463531795));
#27531=CARTESIAN_POINT('Ctrl Pts',(0.0966429852305456,1.,2.14787463531795));
#27532=CARTESIAN_POINT('Ctrl Pts',(0.0994654261990913,-1.,2.14216588396025));
#27533=CARTESIAN_POINT('Ctrl Pts',(0.0994654261990913,1.,2.14216588396025));
#27534=CARTESIAN_POINT('Ctrl Pts',(0.1022477005561,-1.,2.13644992667165));
#27535=CARTESIAN_POINT('Ctrl Pts',(0.1022477005561,1.,2.13644992667165));
#27536=CARTESIAN_POINT('Ctrl Pts',(0.104989479152739,-1.,2.13072704887293));
#27537=CARTESIAN_POINT('Ctrl Pts',(0.104989479152739,1.,2.13072704887293));
#27538=CARTESIAN_POINT('Ctrl Pts',(0.10769043523109,-1.,2.12499752307));
#27539=CARTESIAN_POINT('Ctrl Pts',(0.10769043523109,1.,2.12499752307));
#27540=CARTESIAN_POINT('Ctrl Pts',(0.110350236135025,-1.,2.11926155590865));
#27541=CARTESIAN_POINT('Ctrl Pts',(0.110350236135025,1.,2.11926155590865));
#27542=CARTESIAN_POINT('Ctrl Pts',(0.112968534419737,-1.,2.11351924490306));
#27543=CARTESIAN_POINT('Ctrl Pts',(0.112968534419737,1.,2.11351924490306));
#27544=CARTESIAN_POINT('Ctrl Pts',(0.115544957687926,-1.,2.10777050261309));
#27545=CARTESIAN_POINT('Ctrl Pts',(0.115544957687926,1.,2.10777050261309));
#27546=CARTESIAN_POINT('Ctrl Pts',(0.118079107988355,-1.,2.102015121329));
#27547=CARTESIAN_POINT('Ctrl Pts',(0.118079107988355,1.,2.102015121329));
#27548=CARTESIAN_POINT('Ctrl Pts',(0.120570567965122,-1.,2.0962529286773));
#27549=CARTESIAN_POINT('Ctrl Pts',(0.120570567965122,1.,2.0962529286773));
#27550=CARTESIAN_POINT('Ctrl Pts',(0.123018905621083,-1.,2.09048392424825));
#27551=CARTESIAN_POINT('Ctrl Pts',(0.123018905621083,1.,2.09048392424825));
#27552=CARTESIAN_POINT('Ctrl Pts',(0.125423679412061,-1.,2.08470840653643));
#27553=CARTESIAN_POINT('Ctrl Pts',(0.125423679412061,1.,2.08470840653643));
#27554=CARTESIAN_POINT('Ctrl Pts',(0.12778444527612,-1.,2.07892715110987));
#27555=CARTESIAN_POINT('Ctrl Pts',(0.12778444527612,1.,2.07892715110987));
#27556=CARTESIAN_POINT('Ctrl Pts',(0.130100748328403,-1.,2.07314114713063));
#27557=CARTESIAN_POINT('Ctrl Pts',(0.130100748328403,1.,2.07314114713063));
#27558=CARTESIAN_POINT('Ctrl Pts',(0.13237211154771,-1.,2.06735123910326));
#27559=CARTESIAN_POINT('Ctrl Pts',(0.13237211154771,1.,2.06735123910326));
#27560=CARTESIAN_POINT('Ctrl Pts',(0.134598026192106,-1.,2.06155781517842));
#27561=CARTESIAN_POINT('Ctrl Pts',(0.134598026192106,1.,2.06155781517842));
#27562=CARTESIAN_POINT('Ctrl Pts',(0.136777941218043,-1.,2.05576044414264));
#27563=CARTESIAN_POINT('Ctrl Pts',(0.136777941218043,1.,2.05576044414264));
#27564=CARTESIAN_POINT('Ctrl Pts',(0.138911255368966,-1.,2.04995762001328));
#27565=CARTESIAN_POINT('Ctrl Pts',(0.138911255368966,1.,2.04995762001328));
#27566=CARTESIAN_POINT('Ctrl Pts',(0.140997332152546,-1.,2.04414757947916));
#27567=CARTESIAN_POINT('Ctrl Pts',(0.140997332152546,1.,2.04414757947916));
#27568=CARTESIAN_POINT('Ctrl Pts',(0.143035515058208,-1.,2.03832911025912));
#27569=CARTESIAN_POINT('Ctrl Pts',(0.143035515058208,1.,2.03832911025912));
#27570=CARTESIAN_POINT('Ctrl Pts',(0.145025140186057,-1.,2.03250223739942));
#27571=CARTESIAN_POINT('Ctrl Pts',(0.145025140186057,1.,2.03250223739942));
#27572=CARTESIAN_POINT('Ctrl Pts',(0.146965557332583,-1.,2.02666926182017));
#27573=CARTESIAN_POINT('Ctrl Pts',(0.146965557332583,1.,2.02666926182017));
#27574=CARTESIAN_POINT('Ctrl Pts',(0.148856124775337,-1.,2.02083464969894));
#27575=CARTESIAN_POINT('Ctrl Pts',(0.148856124775337,1.,2.02083464969894));
#27576=CARTESIAN_POINT('Ctrl Pts',(0.150696157673078,-1.,2.01500291940238));
#27577=CARTESIAN_POINT('Ctrl Pts',(0.150696157673078,1.,2.01500291940238));
#27578=CARTESIAN_POINT('Ctrl Pts',(0.152484883621449,-1.,2.00917680318424));
#27579=CARTESIAN_POINT('Ctrl Pts',(0.152484883621449,1.,2.00917680318424));
#27580=CARTESIAN_POINT('Ctrl Pts',(0.154221403049722,-1.,2.00335565310543));
#27581=CARTESIAN_POINT('Ctrl Pts',(0.154221403049722,1.,2.00335565310543));
#27582=CARTESIAN_POINT('Ctrl Pts',(0.155904629548783,-1.,1.99753284771497));
#27583=CARTESIAN_POINT('Ctrl Pts',(0.155904629548783,1.,1.99753284771497));
#27584=CARTESIAN_POINT('Ctrl Pts',(0.157533331459227,-1.,1.99169810931908));
#27585=CARTESIAN_POINT('Ctrl Pts',(0.157533331459227,1.,1.99169810931908));
#27586=CARTESIAN_POINT('Ctrl Pts',(0.159106226437299,-1.,1.98584238283292));
#27587=CARTESIAN_POINT('Ctrl Pts',(0.159106226437299,1.,1.98584238283292));
#27588=CARTESIAN_POINT('Ctrl Pts',(0.160622060784611,-1.,1.97996195437559));
#27589=CARTESIAN_POINT('Ctrl Pts',(0.160622060784611,1.,1.97996195437559));
#27590=CARTESIAN_POINT('Ctrl Pts',(0.162079693556288,-1.,1.97406280235188));
#27591=CARTESIAN_POINT('Ctrl Pts',(0.162079693556288,1.,1.97406280235188));
#27592=CARTESIAN_POINT('Ctrl Pts',(0.163478185457734,-1.,1.96816512677967));
#27593=CARTESIAN_POINT('Ctrl Pts',(0.163478185457734,1.,1.96816512677967));
#27594=CARTESIAN_POINT('Ctrl Pts',(0.164816568920269,-1.,1.96229379940136));
#27595=CARTESIAN_POINT('Ctrl Pts',(0.164816568920269,1.,1.96229379940136));
#27596=CARTESIAN_POINT('Ctrl Pts',(0.166093592002812,-1.,1.9564675971873));
#27597=CARTESIAN_POINT('Ctrl Pts',(0.166093592002812,1.,1.9564675971873));
#27598=CARTESIAN_POINT('Ctrl Pts',(0.167307501784475,-1.,1.95069027794294));
#27599=CARTESIAN_POINT('Ctrl Pts',(0.167307501784475,1.,1.95069027794294));
#27600=CARTESIAN_POINT('Ctrl Pts',(0.168455741607556,-1.,1.94493757756931));
#27601=CARTESIAN_POINT('Ctrl Pts',(0.168455741607556,1.,1.94493757756931));
#27602=CARTESIAN_POINT('Ctrl Pts',(0.16953490481749,-1.,1.93915639211581));
#27603=CARTESIAN_POINT('Ctrl Pts',(0.16953490481749,1.,1.93915639211581));
#27604=CARTESIAN_POINT('Ctrl Pts',(0.170541253116201,-1.,1.93329183155539));
#27605=CARTESIAN_POINT('Ctrl Pts',(0.170541253116201,1.,1.93329183155539));
#27606=CARTESIAN_POINT('Ctrl Pts',(0.171471191532988,-1.,1.92731093582036));
#27607=CARTESIAN_POINT('Ctrl Pts',(0.171471191532988,1.,1.92731093582036));
#27608=CARTESIAN_POINT('Ctrl Pts',(0.172321621259513,-1.,1.9212233439798));
#27609=CARTESIAN_POINT('Ctrl Pts',(0.172321621259513,1.,1.9212233439798));
#27610=CARTESIAN_POINT('Ctrl Pts',(0.173090695383496,-1.,1.91511429159527));
#27611=CARTESIAN_POINT('Ctrl Pts',(0.173090695383496,1.,1.91511429159527));
#27612=CARTESIAN_POINT('Ctrl Pts',(0.173776635257816,-1.,1.90911693975267));
#27613=CARTESIAN_POINT('Ctrl Pts',(0.173776635257816,1.,1.90911693975267));
#27614=CARTESIAN_POINT('Ctrl Pts',(0.174375518661085,-1.,1.90335253862834));
#27615=CARTESIAN_POINT('Ctrl Pts',(0.174375518661085,1.,1.90335253862834));
#27616=CARTESIAN_POINT('Ctrl Pts',(0.174879405091263,-1.,1.89788101117132));
#27617=CARTESIAN_POINT('Ctrl Pts',(0.174879405091263,1.,1.89788101117132));
#27618=CARTESIAN_POINT('Ctrl Pts',(0.175274276190844,-1.,1.892646301985));
#27619=CARTESIAN_POINT('Ctrl Pts',(0.175274276190844,1.,1.892646301985));
#27620=CARTESIAN_POINT('Ctrl Pts',(0.175538155840648,-1.,1.88742606273259));
#27621=CARTESIAN_POINT('Ctrl Pts',(0.175538155840648,1.,1.88742606273259));
#27622=CARTESIAN_POINT('Ctrl Pts',(0.175644148889698,-1.,1.88188663145367));
#27623=CARTESIAN_POINT('Ctrl Pts',(0.175644148889698,1.,1.88188663145367));
#27624=CARTESIAN_POINT('Ctrl Pts',(0.175563480746485,-1.,1.87563767773588));
#27625=CARTESIAN_POINT('Ctrl Pts',(0.175563480746485,1.,1.87563767773588));
#27626=CARTESIAN_POINT('Ctrl Pts',(0.175268337590757,-1.,1.86828349694799));
#27627=CARTESIAN_POINT('Ctrl Pts',(0.175268337590757,1.,1.86828349694799));
#27628=CARTESIAN_POINT('Ctrl Pts',(0.17473525927603,-1.,1.85948367088837));
#27629=CARTESIAN_POINT('Ctrl Pts',(0.17473525927603,1.,1.85948367088837));
#27630=CARTESIAN_POINT('Ctrl Pts',(0.173946627587731,-1.,1.8489811319852));
#27631=CARTESIAN_POINT('Ctrl Pts',(0.173946627587731,1.,1.8489811319852));
#27632=CARTESIAN_POINT('Ctrl Pts',(0.1728894428919,-1.,1.83658380527692));
#27633=CARTESIAN_POINT('Ctrl Pts',(0.1728894428919,1.,1.83658380527692));
#27634=CARTESIAN_POINT('Ctrl Pts',(0.171554770204119,-1.,1.82215766811545));
#27635=CARTESIAN_POINT('Ctrl Pts',(0.171554770204119,1.,1.82215766811545));
#27636=CARTESIAN_POINT('Ctrl Pts',(0.169936923904608,-1.,1.80561530629706));
#27637=CARTESIAN_POINT('Ctrl Pts',(0.169936923904608,1.,1.80561530629706));
#27638=CARTESIAN_POINT('Ctrl Pts',(0.168032772805197,-1.,1.7869064998507));
#27639=CARTESIAN_POINT('Ctrl Pts',(0.168032772805197,1.,1.7869064998507));
#27640=CARTESIAN_POINT('Ctrl Pts',(0.1662793551464,-1.,1.77018771684844));
#27641=CARTESIAN_POINT('Ctrl Pts',(0.1662793551464,1.,1.77018771684844));
#27642=CARTESIAN_POINT('Ctrl Pts',(0.164834765707158,-1.,1.75666056638427));
#27643=CARTESIAN_POINT('Ctrl Pts',(0.164834765707158,1.,1.75666056638427));
#27644=CARTESIAN_POINT('Ctrl Pts',(0.163814161002002,-1.,1.7472034950333));
#27645=CARTESIAN_POINT('Ctrl Pts',(0.163814161002002,1.,1.7472034950333));
#27646=CARTESIAN_POINT('Ctrl Pts',(0.163289472382896,-1.,1.74236521665491));
#27647=CARTESIAN_POINT('Ctrl Pts',(0.163289472382896,1.,1.74236521665491));
#27648=CARTESIAN_POINT('',(0.0694764450219578,1.,2.19890268624765));
#27649=CARTESIAN_POINT('Ctrl Pts',(0.0694764450219578,1.,2.19890268624765));
#27650=CARTESIAN_POINT('Ctrl Pts',(0.0701143536325487,1.,2.19777582085423));
#27651=CARTESIAN_POINT('Ctrl Pts',(0.0713863779526151,1.,2.19552129484002));
#27652=CARTESIAN_POINT('Ctrl Pts',(0.0732830357306722,1.,2.19213712013662));
#27653=CARTESIAN_POINT('Ctrl Pts',(0.0757891465836145,1.,2.1876201139953));
#27654=CARTESIAN_POINT('Ctrl Pts',(0.078883772768524,1.,2.18196589448887));
#27655=CARTESIAN_POINT('Ctrl Pts',(0.0819402680872763,1.,2.176303712113));
#27656=CARTESIAN_POINT('Ctrl Pts',(0.084958462083537,1.,2.17063357870952));
#27657=CARTESIAN_POINT('Ctrl Pts',(0.087938129138692,1.,2.16495552645014));
#27658=CARTESIAN_POINT('Ctrl Pts',(0.0908789888107263,1.,2.15926961544516));
#27659=CARTESIAN_POINT('Ctrl Pts',(0.0937807218867641,1.,2.1535759397817));
#27660=CARTESIAN_POINT('Ctrl Pts',(0.0966429852305456,1.,2.14787463531795));
#27661=CARTESIAN_POINT('Ctrl Pts',(0.0994654261990913,1.,2.14216588396025));
#27662=CARTESIAN_POINT('Ctrl Pts',(0.1022477005561,1.,2.13644992667165));
#27663=CARTESIAN_POINT('Ctrl Pts',(0.104989479152739,1.,2.13072704887293));
#27664=CARTESIAN_POINT('Ctrl Pts',(0.10769043523109,1.,2.12499752307));
#27665=CARTESIAN_POINT('Ctrl Pts',(0.110350236135025,1.,2.11926155590865));
#27666=CARTESIAN_POINT('Ctrl Pts',(0.112968534419737,1.,2.11351924490306));
#27667=CARTESIAN_POINT('Ctrl Pts',(0.115544957687926,1.,2.10777050261309));
#27668=CARTESIAN_POINT('Ctrl Pts',(0.118079107988355,1.,2.102015121329));
#27669=CARTESIAN_POINT('Ctrl Pts',(0.120570567965122,1.,2.0962529286773));
#27670=CARTESIAN_POINT('Ctrl Pts',(0.123018905621083,1.,2.09048392424825));
#27671=CARTESIAN_POINT('Ctrl Pts',(0.125423679412061,1.,2.08470840653643));
#27672=CARTESIAN_POINT('Ctrl Pts',(0.12778444527612,1.,2.07892715110987));
#27673=CARTESIAN_POINT('Ctrl Pts',(0.130100748328403,1.,2.07314114713063));
#27674=CARTESIAN_POINT('Ctrl Pts',(0.13237211154771,1.,2.06735123910326));
#27675=CARTESIAN_POINT('Ctrl Pts',(0.134598026192106,1.,2.06155781517842));
#27676=CARTESIAN_POINT('Ctrl Pts',(0.136777941218043,1.,2.05576044414264));
#27677=CARTESIAN_POINT('Ctrl Pts',(0.138911255368966,1.,2.04995762001328));
#27678=CARTESIAN_POINT('Ctrl Pts',(0.140997332152546,1.,2.04414757947916));
#27679=CARTESIAN_POINT('Ctrl Pts',(0.143035515058208,1.,2.03832911025912));
#27680=CARTESIAN_POINT('Ctrl Pts',(0.145025140186057,1.,2.03250223739942));
#27681=CARTESIAN_POINT('Ctrl Pts',(0.146965557332583,1.,2.02666926182017));
#27682=CARTESIAN_POINT('Ctrl Pts',(0.148856124775337,1.,2.02083464969894));
#27683=CARTESIAN_POINT('Ctrl Pts',(0.150696157673078,1.,2.01500291940238));
#27684=CARTESIAN_POINT('Ctrl Pts',(0.152484883621449,1.,2.00917680318424));
#27685=CARTESIAN_POINT('Ctrl Pts',(0.154221403049722,1.,2.00335565310543));
#27686=CARTESIAN_POINT('Ctrl Pts',(0.155904629548783,1.,1.99753284771497));
#27687=CARTESIAN_POINT('Ctrl Pts',(0.157533331459227,1.,1.99169810931908));
#27688=CARTESIAN_POINT('Ctrl Pts',(0.159106226437299,1.,1.98584238283292));
#27689=CARTESIAN_POINT('Ctrl Pts',(0.160622060784611,1.,1.97996195437559));
#27690=CARTESIAN_POINT('Ctrl Pts',(0.162079693556288,1.,1.97406280235188));
#27691=CARTESIAN_POINT('Ctrl Pts',(0.163478185457734,1.,1.96816512677967));
#27692=CARTESIAN_POINT('Ctrl Pts',(0.164816568920269,1.,1.96229379940136));
#27693=CARTESIAN_POINT('Ctrl Pts',(0.166093592002812,1.,1.9564675971873));
#27694=CARTESIAN_POINT('Ctrl Pts',(0.167307501784475,1.,1.95069027794294));
#27695=CARTESIAN_POINT('Ctrl Pts',(0.168455741607556,1.,1.94493757756931));
#27696=CARTESIAN_POINT('Ctrl Pts',(0.16953490481749,1.,1.93915639211581));
#27697=CARTESIAN_POINT('Ctrl Pts',(0.170541253116201,1.,1.93329183155539));
#27698=CARTESIAN_POINT('Ctrl Pts',(0.171471191532988,1.,1.92731093582036));
#27699=CARTESIAN_POINT('Ctrl Pts',(0.172321621259513,1.,1.9212233439798));
#27700=CARTESIAN_POINT('Ctrl Pts',(0.173090695383496,1.,1.91511429159527));
#27701=CARTESIAN_POINT('Ctrl Pts',(0.173776635257816,1.,1.90911693975267));
#27702=CARTESIAN_POINT('Ctrl Pts',(0.174375518661085,1.,1.90335253862834));
#27703=CARTESIAN_POINT('Ctrl Pts',(0.174879405091263,1.,1.89788101117132));
#27704=CARTESIAN_POINT('Ctrl Pts',(0.175274276190844,1.,1.892646301985));
#27705=CARTESIAN_POINT('Ctrl Pts',(0.175538155840648,1.,1.88742606273259));
#27706=CARTESIAN_POINT('Ctrl Pts',(0.175644148889698,1.,1.88188663145367));
#27707=CARTESIAN_POINT('Ctrl Pts',(0.175563480746485,1.,1.87563767773588));
#27708=CARTESIAN_POINT('Ctrl Pts',(0.175268337590757,1.,1.86828349694799));
#27709=CARTESIAN_POINT('Ctrl Pts',(0.17473525927603,1.,1.85948367088837));
#27710=CARTESIAN_POINT('Ctrl Pts',(0.173946627587731,1.,1.8489811319852));
#27711=CARTESIAN_POINT('Ctrl Pts',(0.1728894428919,1.,1.83658380527692));
#27712=CARTESIAN_POINT('Ctrl Pts',(0.171554770204119,1.,1.82215766811545));
#27713=CARTESIAN_POINT('Ctrl Pts',(0.169936923904608,1.,1.80561530629706));
#27714=CARTESIAN_POINT('Ctrl Pts',(0.168032772805197,1.,1.7869064998507));
#27715=CARTESIAN_POINT('Ctrl Pts',(0.1662793551464,1.,1.77018771684844));
#27716=CARTESIAN_POINT('Ctrl Pts',(0.164834765707158,1.,1.75666056638427));
#27717=CARTESIAN_POINT('Ctrl Pts',(0.163814161002002,1.,1.7472034950333));
#27718=CARTESIAN_POINT('Ctrl Pts',(0.163289472382896,1.,1.74236521665491));
#27719=CARTESIAN_POINT('',(0.0694764450219578,0.,2.19890268624765));
#27720=CARTESIAN_POINT('Origin',(-0.0694764450219586,0.,2.19890268624765));
#27721=CARTESIAN_POINT('',(-0.0694764450219586,1.,2.19890268624765));
#27722=CARTESIAN_POINT('',(0.0694764450219578,1.,2.19890268624765));
#27723=CARTESIAN_POINT('',(-0.0694764450219586,0.,2.19890268624765));
#27724=CARTESIAN_POINT('Ctrl Pts',(-0.163289472382896,-1.,1.74236521665491));
#27725=CARTESIAN_POINT('Ctrl Pts',(-0.163289472382896,1.,1.74236521665491));
#27726=CARTESIAN_POINT('Ctrl Pts',(-0.163814161002474,-1.,1.74720349503904));
#27727=CARTESIAN_POINT('Ctrl Pts',(-0.163814161002474,1.,1.74720349503904));
#27728=CARTESIAN_POINT('Ctrl Pts',(-0.164834765708484,-1.,1.75666056640041));
#27729=CARTESIAN_POINT('Ctrl Pts',(-0.164834765708484,1.,1.75666056640041));
#27730=CARTESIAN_POINT('Ctrl Pts',(-0.166279355148738,-1.,1.77018771687692));
#27731=CARTESIAN_POINT('Ctrl Pts',(-0.166279355148738,1.,1.77018771687692));
#27732=CARTESIAN_POINT('Ctrl Pts',(-0.16803277280837,-1.,1.78690649988931));
#27733=CARTESIAN_POINT('Ctrl Pts',(-0.16803277280837,1.,1.78690649988931));
#27734=CARTESIAN_POINT('Ctrl Pts',(-0.169936923908078,-1.,1.80561530633924));
#27735=CARTESIAN_POINT('Ctrl Pts',(-0.169936923908078,1.,1.80561530633924));
#27736=CARTESIAN_POINT('Ctrl Pts',(-0.171554770207306,-1.,1.82215766815414));
#27737=CARTESIAN_POINT('Ctrl Pts',(-0.171554770207306,1.,1.82215766815414));
#27738=CARTESIAN_POINT('Ctrl Pts',(-0.17288944289442,-1.,1.83658380530747));
#27739=CARTESIAN_POINT('Ctrl Pts',(-0.17288944289442,1.,1.83658380530747));
#27740=CARTESIAN_POINT('Ctrl Pts',(-0.173946627589401,-1.,1.84898113200543));
#27741=CARTESIAN_POINT('Ctrl Pts',(-0.173946627589401,1.,1.84898113200543));
#27742=CARTESIAN_POINT('Ctrl Pts',(-0.174735259276856,-1.,1.85948367089838));
#27743=CARTESIAN_POINT('Ctrl Pts',(-0.174735259276856,1.,1.85948367089838));
#27744=CARTESIAN_POINT('Ctrl Pts',(-0.175268337590901,-1.,1.86828349694972));
#27745=CARTESIAN_POINT('Ctrl Pts',(-0.175268337590901,1.,1.86828349694972));
#27746=CARTESIAN_POINT('Ctrl Pts',(-0.175563480746206,-1.,1.87563767773249));
#27747=CARTESIAN_POINT('Ctrl Pts',(-0.175563480746206,1.,1.87563767773249));
#27748=CARTESIAN_POINT('Ctrl Pts',(-0.175644148889271,-1.,1.88188663144846));
#27749=CARTESIAN_POINT('Ctrl Pts',(-0.175644148889271,1.,1.88188663144846));
#27750=CARTESIAN_POINT('Ctrl Pts',(-0.175538155840286,-1.,1.88742606272818));
#27751=CARTESIAN_POINT('Ctrl Pts',(-0.175538155840286,1.,1.88742606272818));
#27752=CARTESIAN_POINT('Ctrl Pts',(-0.175274276190664,-1.,1.89264630198279));
#27753=CARTESIAN_POINT('Ctrl Pts',(-0.175274276190664,1.,1.89264630198279));
#27754=CARTESIAN_POINT('Ctrl Pts',(-0.174879405091277,-1.,1.89788101117148));
#27755=CARTESIAN_POINT('Ctrl Pts',(-0.174879405091277,1.,1.89788101117148));
#27756=CARTESIAN_POINT('Ctrl Pts',(-0.174375518661222,-1.,1.90335253863003));
#27757=CARTESIAN_POINT('Ctrl Pts',(-0.174375518661222,1.,1.90335253863003));
#27758=CARTESIAN_POINT('Ctrl Pts',(-0.173776635257984,-1.,1.90911693975475));
#27759=CARTESIAN_POINT('Ctrl Pts',(-0.173776635257984,1.,1.90911693975475));
#27760=CARTESIAN_POINT('Ctrl Pts',(-0.173090695383619,-1.,1.91511429159681));
#27761=CARTESIAN_POINT('Ctrl Pts',(-0.173090695383619,1.,1.91511429159681));
#27762=CARTESIAN_POINT('Ctrl Pts',(-0.172321621259557,-1.,1.92122334398034));
#27763=CARTESIAN_POINT('Ctrl Pts',(-0.172321621259557,1.,1.92122334398034));
#27764=CARTESIAN_POINT('Ctrl Pts',(-0.17147119153296,-1.,1.92731093582));
#27765=CARTESIAN_POINT('Ctrl Pts',(-0.17147119153296,1.,1.92731093582));
#27766=CARTESIAN_POINT('Ctrl Pts',(-0.170541253116136,-1.,1.93329183155455));
#27767=CARTESIAN_POINT('Ctrl Pts',(-0.170541253116136,1.,1.93329183155455));
#27768=CARTESIAN_POINT('Ctrl Pts',(-0.169534904817425,-1.,1.93915639211497));
#27769=CARTESIAN_POINT('Ctrl Pts',(-0.169534904817425,1.,1.93915639211497));
#27770=CARTESIAN_POINT('Ctrl Pts',(-0.168455741607516,-1.,1.94493757756879));
#27771=CARTESIAN_POINT('Ctrl Pts',(-0.168455741607516,1.,1.94493757756879));
#27772=CARTESIAN_POINT('Ctrl Pts',(-0.167307501784469,-1.,1.95069027794286));
#27773=CARTESIAN_POINT('Ctrl Pts',(-0.167307501784469,1.,1.95069027794286));
#27774=CARTESIAN_POINT('Ctrl Pts',(-0.166093592002833,-1.,1.95646759718755));
#27775=CARTESIAN_POINT('Ctrl Pts',(-0.166093592002833,1.,1.95646759718755));
#27776=CARTESIAN_POINT('Ctrl Pts',(-0.1648165689203,-1.,1.96229379940174));
#27777=CARTESIAN_POINT('Ctrl Pts',(-0.1648165689203,1.,1.96229379940174));
#27778=CARTESIAN_POINT('Ctrl Pts',(-0.16347818545776,-1.,1.96816512678));
#27779=CARTESIAN_POINT('Ctrl Pts',(-0.16347818545776,1.,1.96816512678));
#27780=CARTESIAN_POINT('Ctrl Pts',(-0.162079693556302,-1.,1.97406280235204));
#27781=CARTESIAN_POINT('Ctrl Pts',(-0.162079693556302,1.,1.97406280235204));
#27782=CARTESIAN_POINT('Ctrl Pts',(-0.16062206078461,-1.,1.97996195437557));
#27783=CARTESIAN_POINT('Ctrl Pts',(-0.16062206078461,1.,1.97996195437557));
#27784=CARTESIAN_POINT('Ctrl Pts',(-0.159106226437289,-1.,1.98584238283279));
#27785=CARTESIAN_POINT('Ctrl Pts',(-0.159106226437289,1.,1.98584238283279));
#27786=CARTESIAN_POINT('Ctrl Pts',(-0.157533331459215,-1.,1.99169810931893));
#27787=CARTESIAN_POINT('Ctrl Pts',(-0.157533331459215,1.,1.99169810931893));
#27788=CARTESIAN_POINT('Ctrl Pts',(-0.155904629548775,-1.,1.99753284771487));
#27789=CARTESIAN_POINT('Ctrl Pts',(-0.155904629548775,1.,1.99753284771487));
#27790=CARTESIAN_POINT('Ctrl Pts',(-0.154221403049719,-1.,2.00335565310539));
#27791=CARTESIAN_POINT('Ctrl Pts',(-0.154221403049719,1.,2.00335565310539));
#27792=CARTESIAN_POINT('Ctrl Pts',(-0.152484883621452,-1.,2.00917680318426));
#27793=CARTESIAN_POINT('Ctrl Pts',(-0.152484883621452,1.,2.00917680318426));
#27794=CARTESIAN_POINT('Ctrl Pts',(-0.150696157673084,-1.,2.01500291940243));
#27795=CARTESIAN_POINT('Ctrl Pts',(-0.150696157673084,1.,2.01500291940243));
#27796=CARTESIAN_POINT('Ctrl Pts',(-0.148856124775343,-1.,2.02083464969897));
#27797=CARTESIAN_POINT('Ctrl Pts',(-0.148856124775343,1.,2.02083464969897));
#27798=CARTESIAN_POINT('Ctrl Pts',(-0.146965557332586,-1.,2.02666926182017));
#27799=CARTESIAN_POINT('Ctrl Pts',(-0.146965557332586,1.,2.02666926182017));
#27800=CARTESIAN_POINT('Ctrl Pts',(-0.145025140186058,-1.,2.03250223739941));
#27801=CARTESIAN_POINT('Ctrl Pts',(-0.145025140186058,1.,2.03250223739941));
#27802=CARTESIAN_POINT('Ctrl Pts',(-0.143035515058208,-1.,2.03832911025913));
#27803=CARTESIAN_POINT('Ctrl Pts',(-0.143035515058208,1.,2.03832911025913));
#27804=CARTESIAN_POINT('Ctrl Pts',(-0.140997332152546,-1.,2.04414757947919));
#27805=CARTESIAN_POINT('Ctrl Pts',(-0.140997332152546,1.,2.04414757947919));
#27806=CARTESIAN_POINT('Ctrl Pts',(-0.138911255368966,-1.,2.04995762001333));
#27807=CARTESIAN_POINT('Ctrl Pts',(-0.138911255368966,1.,2.04995762001333));
#27808=CARTESIAN_POINT('Ctrl Pts',(-0.136777941218044,-1.,2.0557604441427));
#27809=CARTESIAN_POINT('Ctrl Pts',(-0.136777941218044,1.,2.0557604441427));
#27810=CARTESIAN_POINT('Ctrl Pts',(-0.134598026192107,-1.,2.06155781517844));
#27811=CARTESIAN_POINT('Ctrl Pts',(-0.134598026192107,1.,2.06155781517844));
#27812=CARTESIAN_POINT('Ctrl Pts',(-0.13237211154771,-1.,2.06735123910319));
#27813=CARTESIAN_POINT('Ctrl Pts',(-0.13237211154771,1.,2.06735123910319));
#27814=CARTESIAN_POINT('Ctrl Pts',(-0.130100748328401,-1.,2.07314114713047));
#27815=CARTESIAN_POINT('Ctrl Pts',(-0.130100748328401,1.,2.07314114713047));
#27816=CARTESIAN_POINT('Ctrl Pts',(-0.127784445276116,-1.,2.07892715110967));
#27817=CARTESIAN_POINT('Ctrl Pts',(-0.127784445276116,1.,2.07892715110967));
#27818=CARTESIAN_POINT('Ctrl Pts',(-0.125423679412058,-1.,2.08470840653628));
#27819=CARTESIAN_POINT('Ctrl Pts',(-0.125423679412058,1.,2.08470840653628));
#27820=CARTESIAN_POINT('Ctrl Pts',(-0.123018905621083,-1.,2.09048392424826));
#27821=CARTESIAN_POINT('Ctrl Pts',(-0.123018905621083,1.,2.09048392424826));
#27822=CARTESIAN_POINT('Ctrl Pts',(-0.120570567965129,-1.,2.09625292867756));
#27823=CARTESIAN_POINT('Ctrl Pts',(-0.120570567965129,1.,2.09625292867756));
#27824=CARTESIAN_POINT('Ctrl Pts',(-0.118079107988368,-1.,2.10201512132945));
#27825=CARTESIAN_POINT('Ctrl Pts',(-0.118079107988368,1.,2.10201512132945));
#27826=CARTESIAN_POINT('Ctrl Pts',(-0.115544957687941,-1.,2.10777050261359));
#27827=CARTESIAN_POINT('Ctrl Pts',(-0.115544957687941,1.,2.10777050261359));
#27828=CARTESIAN_POINT('Ctrl Pts',(-0.112968534419746,-1.,2.11351924490335));
#27829=CARTESIAN_POINT('Ctrl Pts',(-0.112968534419746,1.,2.11351924490335));
#27830=CARTESIAN_POINT('Ctrl Pts',(-0.11035023613502,-1.,2.11926155590849));
#27831=CARTESIAN_POINT('Ctrl Pts',(-0.11035023613502,1.,2.11926155590849));
#27832=CARTESIAN_POINT('Ctrl Pts',(-0.107690435231068,-1.,2.12499752306927));
#27833=CARTESIAN_POINT('Ctrl Pts',(-0.107690435231068,1.,2.12499752306927));
#27834=CARTESIAN_POINT('Ctrl Pts',(-0.104989479152703,-1.,2.1307270488718));
#27835=CARTESIAN_POINT('Ctrl Pts',(-0.104989479152703,1.,2.1307270488718));
#27836=CARTESIAN_POINT('Ctrl Pts',(-0.102247700556064,-1.,2.13644992667052));
#27837=CARTESIAN_POINT('Ctrl Pts',(-0.102247700556064,1.,2.13644992667052));
#27838=CARTESIAN_POINT('Ctrl Pts',(-0.0994654261990745,-1.,2.14216588395974));
#27839=CARTESIAN_POINT('Ctrl Pts',(-0.0994654261990745,1.,2.14216588395974));
#27840=CARTESIAN_POINT('Ctrl Pts',(-0.0966429852305691,-1.,2.14787463531864));
#27841=CARTESIAN_POINT('Ctrl Pts',(-0.0966429852305691,1.,2.14787463531864));
#27842=CARTESIAN_POINT('Ctrl Pts',(-0.0937807218868348,-1.,2.15357593978377));
#27843=CARTESIAN_POINT('Ctrl Pts',(-0.0937807218868348,1.,2.15357593978377));
#27844=CARTESIAN_POINT('Ctrl Pts',(-0.0908789888108269,-1.,2.15926961544808));
#27845=CARTESIAN_POINT('Ctrl Pts',(-0.0908789888108269,1.,2.15926961544808));
#27846=CARTESIAN_POINT('Ctrl Pts',(-0.0879381291387825,-1.,2.16495552645275));
#27847=CARTESIAN_POINT('Ctrl Pts',(-0.0879381291387825,1.,2.16495552645275));
#27848=CARTESIAN_POINT('Ctrl Pts',(-0.0849584620835646,-1.,2.17063357871031));
#27849=CARTESIAN_POINT('Ctrl Pts',(-0.0849584620835646,1.,2.17063357871031));
#27850=CARTESIAN_POINT('Ctrl Pts',(-0.0819402680871942,-1.,2.1763037121106));
#27851=CARTESIAN_POINT('Ctrl Pts',(-0.0819402680871942,1.,2.1763037121106));
#27852=CARTESIAN_POINT('Ctrl Pts',(-0.078883772768323,-1.,2.18196589448304));
#27853=CARTESIAN_POINT('Ctrl Pts',(-0.078883772768323,1.,2.18196589448304));
#27854=CARTESIAN_POINT('Ctrl Pts',(-0.0757891465833414,-1.,2.1876201139874));
#27855=CARTESIAN_POINT('Ctrl Pts',(-0.0757891465833414,1.,2.1876201139874));
#27856=CARTESIAN_POINT('Ctrl Pts',(-0.0732830357304279,-1.,2.19213712012956));
#27857=CARTESIAN_POINT('Ctrl Pts',(-0.0732830357304279,1.,2.19213712012956));
#27858=CARTESIAN_POINT('Ctrl Pts',(-0.071386377952463,-1.,2.19552129483562));
#27859=CARTESIAN_POINT('Ctrl Pts',(-0.071386377952463,1.,2.19552129483562));
#27860=CARTESIAN_POINT('Ctrl Pts',(-0.0701143536324929,-1.,2.19777582085261));
#27861=CARTESIAN_POINT('Ctrl Pts',(-0.0701143536324929,1.,2.19777582085261));
#27862=CARTESIAN_POINT('Ctrl Pts',(-0.0694764450219586,-1.,2.19890268624765));
#27863=CARTESIAN_POINT('Ctrl Pts',(-0.0694764450219586,1.,2.19890268624765));
#27864=CARTESIAN_POINT('',(-0.163289472382896,1.,1.74236521665491));
#27865=CARTESIAN_POINT('Ctrl Pts',(-0.163289472382896,1.,1.74236521665491));
#27866=CARTESIAN_POINT('Ctrl Pts',(-0.163814161002474,1.,1.74720349503904));
#27867=CARTESIAN_POINT('Ctrl Pts',(-0.164834765708484,1.,1.75666056640041));
#27868=CARTESIAN_POINT('Ctrl Pts',(-0.166279355148738,1.,1.77018771687692));
#27869=CARTESIAN_POINT('Ctrl Pts',(-0.16803277280837,1.,1.78690649988931));
#27870=CARTESIAN_POINT('Ctrl Pts',(-0.169936923908078,1.,1.80561530633924));
#27871=CARTESIAN_POINT('Ctrl Pts',(-0.171554770207306,1.,1.82215766815414));
#27872=CARTESIAN_POINT('Ctrl Pts',(-0.17288944289442,1.,1.83658380530747));
#27873=CARTESIAN_POINT('Ctrl Pts',(-0.173946627589401,1.,1.84898113200543));
#27874=CARTESIAN_POINT('Ctrl Pts',(-0.174735259276856,1.,1.85948367089838));
#27875=CARTESIAN_POINT('Ctrl Pts',(-0.175268337590901,1.,1.86828349694972));
#27876=CARTESIAN_POINT('Ctrl Pts',(-0.175563480746206,1.,1.87563767773249));
#27877=CARTESIAN_POINT('Ctrl Pts',(-0.175644148889271,1.,1.88188663144846));
#27878=CARTESIAN_POINT('Ctrl Pts',(-0.175538155840286,1.,1.88742606272818));
#27879=CARTESIAN_POINT('Ctrl Pts',(-0.175274276190664,1.,1.89264630198279));
#27880=CARTESIAN_POINT('Ctrl Pts',(-0.174879405091277,1.,1.89788101117148));
#27881=CARTESIAN_POINT('Ctrl Pts',(-0.174375518661222,1.,1.90335253863003));
#27882=CARTESIAN_POINT('Ctrl Pts',(-0.173776635257984,1.,1.90911693975475));
#27883=CARTESIAN_POINT('Ctrl Pts',(-0.173090695383619,1.,1.91511429159681));
#27884=CARTESIAN_POINT('Ctrl Pts',(-0.172321621259557,1.,1.92122334398034));
#27885=CARTESIAN_POINT('Ctrl Pts',(-0.17147119153296,1.,1.92731093582));
#27886=CARTESIAN_POINT('Ctrl Pts',(-0.170541253116136,1.,1.93329183155455));
#27887=CARTESIAN_POINT('Ctrl Pts',(-0.169534904817425,1.,1.93915639211497));
#27888=CARTESIAN_POINT('Ctrl Pts',(-0.168455741607516,1.,1.94493757756879));
#27889=CARTESIAN_POINT('Ctrl Pts',(-0.167307501784469,1.,1.95069027794286));
#27890=CARTESIAN_POINT('Ctrl Pts',(-0.166093592002833,1.,1.95646759718755));
#27891=CARTESIAN_POINT('Ctrl Pts',(-0.1648165689203,1.,1.96229379940174));
#27892=CARTESIAN_POINT('Ctrl Pts',(-0.16347818545776,1.,1.96816512678));
#27893=CARTESIAN_POINT('Ctrl Pts',(-0.162079693556302,1.,1.97406280235204));
#27894=CARTESIAN_POINT('Ctrl Pts',(-0.16062206078461,1.,1.97996195437557));
#27895=CARTESIAN_POINT('Ctrl Pts',(-0.159106226437289,1.,1.98584238283279));
#27896=CARTESIAN_POINT('Ctrl Pts',(-0.157533331459215,1.,1.99169810931893));
#27897=CARTESIAN_POINT('Ctrl Pts',(-0.155904629548775,1.,1.99753284771487));
#27898=CARTESIAN_POINT('Ctrl Pts',(-0.154221403049719,1.,2.00335565310539));
#27899=CARTESIAN_POINT('Ctrl Pts',(-0.152484883621452,1.,2.00917680318426));
#27900=CARTESIAN_POINT('Ctrl Pts',(-0.150696157673084,1.,2.01500291940243));
#27901=CARTESIAN_POINT('Ctrl Pts',(-0.148856124775343,1.,2.02083464969897));
#27902=CARTESIAN_POINT('Ctrl Pts',(-0.146965557332586,1.,2.02666926182017));
#27903=CARTESIAN_POINT('Ctrl Pts',(-0.145025140186058,1.,2.03250223739941));
#27904=CARTESIAN_POINT('Ctrl Pts',(-0.143035515058208,1.,2.03832911025913));
#27905=CARTESIAN_POINT('Ctrl Pts',(-0.140997332152546,1.,2.04414757947919));
#27906=CARTESIAN_POINT('Ctrl Pts',(-0.138911255368966,1.,2.04995762001333));
#27907=CARTESIAN_POINT('Ctrl Pts',(-0.136777941218044,1.,2.0557604441427));
#27908=CARTESIAN_POINT('Ctrl Pts',(-0.134598026192107,1.,2.06155781517844));
#27909=CARTESIAN_POINT('Ctrl Pts',(-0.13237211154771,1.,2.06735123910319));
#27910=CARTESIAN_POINT('Ctrl Pts',(-0.130100748328401,1.,2.07314114713047));
#27911=CARTESIAN_POINT('Ctrl Pts',(-0.127784445276116,1.,2.07892715110967));
#27912=CARTESIAN_POINT('Ctrl Pts',(-0.125423679412058,1.,2.08470840653628));
#27913=CARTESIAN_POINT('Ctrl Pts',(-0.123018905621083,1.,2.09048392424826));
#27914=CARTESIAN_POINT('Ctrl Pts',(-0.120570567965129,1.,2.09625292867756));
#27915=CARTESIAN_POINT('Ctrl Pts',(-0.118079107988368,1.,2.10201512132945));
#27916=CARTESIAN_POINT('Ctrl Pts',(-0.115544957687941,1.,2.10777050261359));
#27917=CARTESIAN_POINT('Ctrl Pts',(-0.112968534419746,1.,2.11351924490335));
#27918=CARTESIAN_POINT('Ctrl Pts',(-0.11035023613502,1.,2.11926155590849));
#27919=CARTESIAN_POINT('Ctrl Pts',(-0.107690435231068,1.,2.12499752306927));
#27920=CARTESIAN_POINT('Ctrl Pts',(-0.104989479152703,1.,2.1307270488718));
#27921=CARTESIAN_POINT('Ctrl Pts',(-0.102247700556064,1.,2.13644992667052));
#27922=CARTESIAN_POINT('Ctrl Pts',(-0.0994654261990745,1.,2.14216588395974));
#27923=CARTESIAN_POINT('Ctrl Pts',(-0.0966429852305691,1.,2.14787463531864));
#27924=CARTESIAN_POINT('Ctrl Pts',(-0.0937807218868348,1.,2.15357593978377));
#27925=CARTESIAN_POINT('Ctrl Pts',(-0.0908789888108269,1.,2.15926961544808));
#27926=CARTESIAN_POINT('Ctrl Pts',(-0.0879381291387825,1.,2.16495552645275));
#27927=CARTESIAN_POINT('Ctrl Pts',(-0.0849584620835646,1.,2.17063357871031));
#27928=CARTESIAN_POINT('Ctrl Pts',(-0.0819402680871942,1.,2.1763037121106));
#27929=CARTESIAN_POINT('Ctrl Pts',(-0.078883772768323,1.,2.18196589448304));
#27930=CARTESIAN_POINT('Ctrl Pts',(-0.0757891465833414,1.,2.1876201139874));
#27931=CARTESIAN_POINT('Ctrl Pts',(-0.0732830357304279,1.,2.19213712012956));
#27932=CARTESIAN_POINT('Ctrl Pts',(-0.071386377952463,1.,2.19552129483562));
#27933=CARTESIAN_POINT('Ctrl Pts',(-0.0701143536324929,1.,2.19777582085261));
#27934=CARTESIAN_POINT('Ctrl Pts',(-0.0694764450219586,1.,2.19890268624765));
#27935=CARTESIAN_POINT('',(-0.163289472382897,0.,1.74236521665491));
#27936=CARTESIAN_POINT('Origin',(0.,0.,0.));
#27937=CARTESIAN_POINT('',(-0.383122945602004,1.,1.7075470150345));
#27938=CARTESIAN_POINT('Origin',(0.,1.,0.));
#27939=CARTESIAN_POINT('',(-0.383122945602004,0.,1.7075470150345));
#27940=CARTESIAN_POINT('Ctrl Pts',(-0.61342227326009,-1.,2.11275013067528));
#27941=CARTESIAN_POINT('Ctrl Pts',(-0.61342227326009,1.,2.11275013067528));
#27942=CARTESIAN_POINT('Ctrl Pts',(-0.61246736556225,-1.,2.11187554260142));
#27943=CARTESIAN_POINT('Ctrl Pts',(-0.61246736556225,1.,2.11187554260142));
#27944=CARTESIAN_POINT('Ctrl Pts',(-0.610560911691113,-1.,2.11012443807661));
#27945=CARTESIAN_POINT('Ctrl Pts',(-0.610560911691113,1.,2.11012443807661));
#27946=CARTESIAN_POINT('Ctrl Pts',(-0.607711315456826,-1.,2.10749199615859));
#27947=CARTESIAN_POINT('Ctrl Pts',(-0.607711315456826,1.,2.10749199615859));
#27948=CARTESIAN_POINT('Ctrl Pts',(-0.603932030738212,-1.,2.10397049887709));
#27949=CARTESIAN_POINT('Ctrl Pts',(-0.603932030738212,1.,2.10397049887709));
#27950=CARTESIAN_POINT('Ctrl Pts',(-0.599241616422144,-1.,2.09954930865331));
#27951=CARTESIAN_POINT('Ctrl Pts',(-0.599241616422144,1.,2.09954930865331));
#27952=CARTESIAN_POINT('Ctrl Pts',(-0.594585006052824,-1.,2.09510876220501));
#27953=CARTESIAN_POINT('Ctrl Pts',(-0.594585006052824,1.,2.09510876220501));
#27954=CARTESIAN_POINT('Ctrl Pts',(-0.589962365403189,-1.,2.09064881812053));
#27955=CARTESIAN_POINT('Ctrl Pts',(-0.589962365403189,1.,2.09064881812053));
#27956=CARTESIAN_POINT('Ctrl Pts',(-0.585373918990895,-1.,2.086169437277));
#27957=CARTESIAN_POINT('Ctrl Pts',(-0.585373918990895,1.,2.086169437277));
#27958=CARTESIAN_POINT('Ctrl Pts',(-0.580819952107257,-1.,2.08167059018138));
#27959=CARTESIAN_POINT('Ctrl Pts',(-0.580819952107257,1.,2.08167059018138));
#27960=CARTESIAN_POINT('Ctrl Pts',(-0.576300797416275,-1.,2.07715226767361));
#27961=CARTESIAN_POINT('Ctrl Pts',(-0.576300797416275,1.,2.07715226767361));
#27962=CARTESIAN_POINT('Ctrl Pts',(-0.571816823242411,-1.,2.07261449292757));
#27963=CARTESIAN_POINT('Ctrl Pts',(-0.571816823242411,1.,2.07261449292757));
#27964=CARTESIAN_POINT('Ctrl Pts',(-0.567368421181229,-1.,2.06805732997383));
#27965=CARTESIAN_POINT('Ctrl Pts',(-0.567368421181229,1.,2.06805732997383));
#27966=CARTESIAN_POINT('Ctrl Pts',(-0.562955993082574,-1.,2.06348090160697));
#27967=CARTESIAN_POINT('Ctrl Pts',(-0.562955993082574,1.,2.06348090160697));
#27968=CARTESIAN_POINT('Ctrl Pts',(-0.558579940185467,-1.,2.05888537756571));
#27969=CARTESIAN_POINT('Ctrl Pts',(-0.558579940185467,1.,2.05888537756571));
#27970=CARTESIAN_POINT('Ctrl Pts',(-0.55424065746411,-1.,2.05427091604482));
#27971=CARTESIAN_POINT('Ctrl Pts',(-0.55424065746411,1.,2.05427091604482));
#27972=CARTESIAN_POINT('Ctrl Pts',(-0.549938525150342,-1.,2.04963761077974));
#27973=CARTESIAN_POINT('Ctrl Pts',(-0.549938525150342,1.,2.04963761077974));
#27974=CARTESIAN_POINT('Ctrl Pts',(-0.545673903817348,-1.,2.0449854471456));
#27975=CARTESIAN_POINT('Ctrl Pts',(-0.545673903817348,1.,2.0449854471456));
#27976=CARTESIAN_POINT('Ctrl Pts',(-0.54144712061552,-1.,2.0403142269048));
#27977=CARTESIAN_POINT('Ctrl Pts',(-0.54144712061552,1.,2.0403142269048));
#27978=CARTESIAN_POINT('Ctrl Pts',(-0.537258489833134,-1.,2.03562362953993));
#27979=CARTESIAN_POINT('Ctrl Pts',(-0.537258489833134,1.,2.03562362953993));
#27980=CARTESIAN_POINT('Ctrl Pts',(-0.533108355132905,-1.,2.03091336214401));
#27981=CARTESIAN_POINT('Ctrl Pts',(-0.533108355132905,1.,2.03091336214401));
#27982=CARTESIAN_POINT('Ctrl Pts',(-0.528997127241911,-1.,2.02618329083289));
#27983=CARTESIAN_POINT('Ctrl Pts',(-0.528997127241911,1.,2.02618329083289));
#27984=CARTESIAN_POINT('Ctrl Pts',(-0.524925318333518,-1.,2.02143356304712));
#27985=CARTESIAN_POINT('Ctrl Pts',(-0.524925318333518,1.,2.02143356304712));
#27986=CARTESIAN_POINT('Ctrl Pts',(-0.520893590399428,-1.,2.01666477917305));
#27987=CARTESIAN_POINT('Ctrl Pts',(-0.520893590399428,1.,2.01666477917305));
#27988=CARTESIAN_POINT('Ctrl Pts',(-0.516902681728733,-1.,2.01187773939257));
#27989=CARTESIAN_POINT('Ctrl Pts',(-0.516902681728733,1.,2.01187773939257));
#27990=CARTESIAN_POINT('Ctrl Pts',(-0.512953306961814,-1.,2.00707309946955));
#27991=CARTESIAN_POINT('Ctrl Pts',(-0.512953306961814,1.,2.00707309946955));
#27992=CARTESIAN_POINT('Ctrl Pts',(-0.509046069886152,-1.,2.00225107134733));
#27993=CARTESIAN_POINT('Ctrl Pts',(-0.509046069886152,1.,2.00225107134733));
#27994=CARTESIAN_POINT('Ctrl Pts',(-0.505181361323011,-1.,1.99741107463567));
#27995=CARTESIAN_POINT('Ctrl Pts',(-0.505181361323011,1.,1.99741107463567));
#27996=CARTESIAN_POINT('Ctrl Pts',(-0.501359287727129,-1.,1.9925514912615));
#27997=CARTESIAN_POINT('Ctrl Pts',(-0.501359287727129,1.,1.9925514912615));
#27998=CARTESIAN_POINT('Ctrl Pts',(-0.497579909545564,-1.,1.98767044752929));
#27999=CARTESIAN_POINT('Ctrl Pts',(-0.497579909545564,1.,1.98767044752929));
#28000=CARTESIAN_POINT('Ctrl Pts',(-0.493843476541492,-1.,1.9827665876182));
#28001=CARTESIAN_POINT('Ctrl Pts',(-0.493843476541492,1.,1.9827665876182));
#28002=CARTESIAN_POINT('Ctrl Pts',(-0.490150627860955,-1.,1.97783973019229));
#28003=CARTESIAN_POINT('Ctrl Pts',(-0.490150627860955,1.,1.97783973019229));
#28004=CARTESIAN_POINT('Ctrl Pts',(-0.486502692907661,-1.,1.97289186263272));
#28005=CARTESIAN_POINT('Ctrl Pts',(-0.486502692907661,1.,1.97289186263272));
#28006=CARTESIAN_POINT('Ctrl Pts',(-0.482901662120687,-1.,1.96792703422358));
#28007=CARTESIAN_POINT('Ctrl Pts',(-0.482901662120687,1.,1.96792703422358));
#28008=CARTESIAN_POINT('Ctrl Pts',(-0.479349583074846,-1.,1.96294933055938));
#28009=CARTESIAN_POINT('Ctrl Pts',(-0.479349583074846,1.,1.96294933055938));
#28010=CARTESIAN_POINT('Ctrl Pts',(-0.475848034683172,-1.,1.95796111148175));
#28011=CARTESIAN_POINT('Ctrl Pts',(-0.475848034683172,1.,1.95796111148175));
#28012=CARTESIAN_POINT('Ctrl Pts',(-0.47239767226408,-1.,1.95296148278136));
#28013=CARTESIAN_POINT('Ctrl Pts',(-0.47239767226408,1.,1.95296148278136));
#28014=CARTESIAN_POINT('Ctrl Pts',(-0.468997482913158,-1.,1.94794381136524));
#28015=CARTESIAN_POINT('Ctrl Pts',(-0.468997482913158,1.,1.94794381136524));
#28016=CARTESIAN_POINT('Ctrl Pts',(-0.465645462026065,-1.,1.94289794196205));
#28017=CARTESIAN_POINT('Ctrl Pts',(-0.465645462026065,1.,1.94289794196205));
#28018=CARTESIAN_POINT('Ctrl Pts',(-0.462340031009087,-1.,1.93781486640834));
#28019=CARTESIAN_POINT('Ctrl Pts',(-0.462340031009087,1.,1.93781486640834));
#28020=CARTESIAN_POINT('Ctrl Pts',(-0.459081234547931,-1.,1.93269066517936));
#28021=CARTESIAN_POINT('Ctrl Pts',(-0.459081234547931,1.,1.93269066517936));
#28022=CARTESIAN_POINT('Ctrl Pts',(-0.455872005174335,-1.,1.92753067150461));
#28023=CARTESIAN_POINT('Ctrl Pts',(-0.455872005174335,1.,1.92753067150461));
#28024=CARTESIAN_POINT('Ctrl Pts',(-0.452719478359356,-1.,1.9223538064847));
#28025=CARTESIAN_POINT('Ctrl Pts',(-0.452719478359356,1.,1.9223538064847));
#28026=CARTESIAN_POINT('Ctrl Pts',(-0.449632260106572,-1.,1.91718342555717));
#28027=CARTESIAN_POINT('Ctrl Pts',(-0.449632260106572,1.,1.91718342555717));
#28028=CARTESIAN_POINT('Ctrl Pts',(-0.446617343485651,-1.,1.91203699981095));
#28029=CARTESIAN_POINT('Ctrl Pts',(-0.446617343485651,1.,1.91203699981095));
#28030=CARTESIAN_POINT('Ctrl Pts',(-0.44367755684917,-1.,1.90691756144906));
#28031=CARTESIAN_POINT('Ctrl Pts',(-0.44367755684917,1.,1.90691756144906));
#28032=CARTESIAN_POINT('Ctrl Pts',(-0.440807833704161,-1.,1.90180124389137));
#28033=CARTESIAN_POINT('Ctrl Pts',(-0.440807833704161,1.,1.90180124389137));
#28034=CARTESIAN_POINT('Ctrl Pts',(-0.437995003948443,-1.,1.89663648956549));
#28035=CARTESIAN_POINT('Ctrl Pts',(-0.437995003948443,1.,1.89663648956549));
#28036=CARTESIAN_POINT('Ctrl Pts',(-0.43522566096358,-1.,1.89136993975585));
#28037=CARTESIAN_POINT('Ctrl Pts',(-0.43522566096358,1.,1.89136993975585));
#28038=CARTESIAN_POINT('Ctrl Pts',(-0.432493038548833,-1.,1.88596913666828));
#28039=CARTESIAN_POINT('Ctrl Pts',(-0.432493038548833,1.,1.88596913666828));
#28040=CARTESIAN_POINT('Ctrl Pts',(-0.429803062482217,-1.,1.88044229001778));
#28041=CARTESIAN_POINT('Ctrl Pts',(-0.429803062482217,1.,1.88044229001778));
#28042=CARTESIAN_POINT('Ctrl Pts',(-0.427183828518743,-1.,1.87486989291333));
#28043=CARTESIAN_POINT('Ctrl Pts',(-0.427183828518743,1.,1.87486989291333));
#28044=CARTESIAN_POINT('Ctrl Pts',(-0.424678177290876,-1.,1.8693780394412));
#28045=CARTESIAN_POINT('Ctrl Pts',(-0.424678177290876,1.,1.8693780394412));
#28046=CARTESIAN_POINT('Ctrl Pts',(-0.422327307417885,-1.,1.86408083333863));
#28047=CARTESIAN_POINT('Ctrl Pts',(-0.422327307417885,1.,1.86408083333863));
#28048=CARTESIAN_POINT('Ctrl Pts',(-0.420157287975583,-1.,1.8590328109667));
#28049=CARTESIAN_POINT('Ctrl Pts',(-0.420157287975583,1.,1.8590328109667));
#28050=CARTESIAN_POINT('Ctrl Pts',(-0.418164129144045,-1.,1.8541763285645));
#28051=CARTESIAN_POINT('Ctrl Pts',(-0.418164129144045,1.,1.8541763285645));
#28052=CARTESIAN_POINT('Ctrl Pts',(-0.416300022039885,-1.,1.84929312930314));
#28053=CARTESIAN_POINT('Ctrl Pts',(-0.416300022039885,1.,1.84929312930314));
#28054=CARTESIAN_POINT('Ctrl Pts',(-0.414487438255542,-1.,1.84405757074218));
#28055=CARTESIAN_POINT('Ctrl Pts',(-0.414487438255542,1.,1.84405757074218));
#28056=CARTESIAN_POINT('Ctrl Pts',(-0.412633125322945,-1.,1.8380895347617));
#28057=CARTESIAN_POINT('Ctrl Pts',(-0.412633125322945,1.,1.8380895347617));
#28058=CARTESIAN_POINT('Ctrl Pts',(-0.410641256301276,-1.,1.83100408895047));
#28059=CARTESIAN_POINT('Ctrl Pts',(-0.410641256301276,1.,1.83100408895047));
#28060=CARTESIAN_POINT('Ctrl Pts',(-0.408428948106227,-1.,1.82247022677562));
#28061=CARTESIAN_POINT('Ctrl Pts',(-0.408428948106227,1.,1.82247022677562));
#28062=CARTESIAN_POINT('Ctrl Pts',(-0.405933518407175,-1.,1.81223801812013));
#28063=CARTESIAN_POINT('Ctrl Pts',(-0.405933518407175,1.,1.81223801812013));
#28064=CARTESIAN_POINT('Ctrl Pts',(-0.403107976163396,-1.,1.80012077173238));
#28065=CARTESIAN_POINT('Ctrl Pts',(-0.403107976163396,1.,1.80012077173238));
#28066=CARTESIAN_POINT('Ctrl Pts',(-0.399919403774155,-1.,1.78598826343754));
#28067=CARTESIAN_POINT('Ctrl Pts',(-0.399919403774155,1.,1.78598826343754));
#28068=CARTESIAN_POINT('Ctrl Pts',(-0.396346196110688,-1.,1.76975560043442));
#28069=CARTESIAN_POINT('Ctrl Pts',(-0.396346196110688,1.,1.76975560043442));
#28070=CARTESIAN_POINT('Ctrl Pts',(-0.392375812285395,-1.,1.75137405310193));
#28071=CARTESIAN_POINT('Ctrl Pts',(-0.392375812285395,1.,1.75137405310193));
#28072=CARTESIAN_POINT('Ctrl Pts',(-0.388877023502615,-1.,1.73493170972829));
#28073=CARTESIAN_POINT('Ctrl Pts',(-0.388877023502615,1.,1.73493170972829));
#28074=CARTESIAN_POINT('Ctrl Pts',(-0.386070790323281,-1.,1.72162022244582));
#28075=CARTESIAN_POINT('Ctrl Pts',(-0.386070790323281,1.,1.72162022244582));
#28076=CARTESIAN_POINT('Ctrl Pts',(-0.384119047314215,-1.,1.71231062891398));
#28077=CARTESIAN_POINT('Ctrl Pts',(-0.384119047314215,1.,1.71231062891398));
#28078=CARTESIAN_POINT('Ctrl Pts',(-0.383122945602004,-1.,1.7075470150345));
#28079=CARTESIAN_POINT('Ctrl Pts',(-0.383122945602004,1.,1.7075470150345));
#28080=CARTESIAN_POINT('',(-0.61342227326009,1.,2.11275013067528));
#28081=CARTESIAN_POINT('Ctrl Pts',(-0.61342227326009,1.,2.11275013067528));
#28082=CARTESIAN_POINT('Ctrl Pts',(-0.61246736556225,1.,2.11187554260142));
#28083=CARTESIAN_POINT('Ctrl Pts',(-0.610560911691113,1.,2.11012443807661));
#28084=CARTESIAN_POINT('Ctrl Pts',(-0.607711315456826,1.,2.10749199615859));
#28085=CARTESIAN_POINT('Ctrl Pts',(-0.603932030738212,1.,2.10397049887709));
#28086=CARTESIAN_POINT('Ctrl Pts',(-0.599241616422144,1.,2.09954930865331));
#28087=CARTESIAN_POINT('Ctrl Pts',(-0.594585006052824,1.,2.09510876220501));
#28088=CARTESIAN_POINT('Ctrl Pts',(-0.589962365403189,1.,2.09064881812053));
#28089=CARTESIAN_POINT('Ctrl Pts',(-0.585373918990895,1.,2.086169437277));
#28090=CARTESIAN_POINT('Ctrl Pts',(-0.580819952107257,1.,2.08167059018138));
#28091=CARTESIAN_POINT('Ctrl Pts',(-0.576300797416275,1.,2.07715226767361));
#28092=CARTESIAN_POINT('Ctrl Pts',(-0.571816823242411,1.,2.07261449292757));
#28093=CARTESIAN_POINT('Ctrl Pts',(-0.567368421181229,1.,2.06805732997383));
#28094=CARTESIAN_POINT('Ctrl Pts',(-0.562955993082574,1.,2.06348090160697));
#28095=CARTESIAN_POINT('Ctrl Pts',(-0.558579940185467,1.,2.05888537756571));
#28096=CARTESIAN_POINT('Ctrl Pts',(-0.55424065746411,1.,2.05427091604482));
#28097=CARTESIAN_POINT('Ctrl Pts',(-0.549938525150342,1.,2.04963761077974));
#28098=CARTESIAN_POINT('Ctrl Pts',(-0.545673903817348,1.,2.0449854471456));
#28099=CARTESIAN_POINT('Ctrl Pts',(-0.54144712061552,1.,2.0403142269048));
#28100=CARTESIAN_POINT('Ctrl Pts',(-0.537258489833134,1.,2.03562362953993));
#28101=CARTESIAN_POINT('Ctrl Pts',(-0.533108355132905,1.,2.03091336214401));
#28102=CARTESIAN_POINT('Ctrl Pts',(-0.528997127241911,1.,2.02618329083289));
#28103=CARTESIAN_POINT('Ctrl Pts',(-0.524925318333518,1.,2.02143356304712));
#28104=CARTESIAN_POINT('Ctrl Pts',(-0.520893590399428,1.,2.01666477917305));
#28105=CARTESIAN_POINT('Ctrl Pts',(-0.516902681728733,1.,2.01187773939257));
#28106=CARTESIAN_POINT('Ctrl Pts',(-0.512953306961814,1.,2.00707309946955));
#28107=CARTESIAN_POINT('Ctrl Pts',(-0.509046069886152,1.,2.00225107134733));
#28108=CARTESIAN_POINT('Ctrl Pts',(-0.505181361323011,1.,1.99741107463567));
#28109=CARTESIAN_POINT('Ctrl Pts',(-0.501359287727129,1.,1.9925514912615));
#28110=CARTESIAN_POINT('Ctrl Pts',(-0.497579909545564,1.,1.98767044752929));
#28111=CARTESIAN_POINT('Ctrl Pts',(-0.493843476541492,1.,1.9827665876182));
#28112=CARTESIAN_POINT('Ctrl Pts',(-0.490150627860955,1.,1.97783973019229));
#28113=CARTESIAN_POINT('Ctrl Pts',(-0.486502692907661,1.,1.97289186263272));
#28114=CARTESIAN_POINT('Ctrl Pts',(-0.482901662120687,1.,1.96792703422358));
#28115=CARTESIAN_POINT('Ctrl Pts',(-0.479349583074846,1.,1.96294933055938));
#28116=CARTESIAN_POINT('Ctrl Pts',(-0.475848034683172,1.,1.95796111148175));
#28117=CARTESIAN_POINT('Ctrl Pts',(-0.47239767226408,1.,1.95296148278136));
#28118=CARTESIAN_POINT('Ctrl Pts',(-0.468997482913158,1.,1.94794381136524));
#28119=CARTESIAN_POINT('Ctrl Pts',(-0.465645462026065,1.,1.94289794196205));
#28120=CARTESIAN_POINT('Ctrl Pts',(-0.462340031009087,1.,1.93781486640834));
#28121=CARTESIAN_POINT('Ctrl Pts',(-0.459081234547931,1.,1.93269066517936));
#28122=CARTESIAN_POINT('Ctrl Pts',(-0.455872005174335,1.,1.92753067150461));
#28123=CARTESIAN_POINT('Ctrl Pts',(-0.452719478359356,1.,1.9223538064847));
#28124=CARTESIAN_POINT('Ctrl Pts',(-0.449632260106572,1.,1.91718342555717));
#28125=CARTESIAN_POINT('Ctrl Pts',(-0.446617343485651,1.,1.91203699981095));
#28126=CARTESIAN_POINT('Ctrl Pts',(-0.44367755684917,1.,1.90691756144906));
#28127=CARTESIAN_POINT('Ctrl Pts',(-0.440807833704161,1.,1.90180124389137));
#28128=CARTESIAN_POINT('Ctrl Pts',(-0.437995003948443,1.,1.89663648956549));
#28129=CARTESIAN_POINT('Ctrl Pts',(-0.43522566096358,1.,1.89136993975585));
#28130=CARTESIAN_POINT('Ctrl Pts',(-0.432493038548833,1.,1.88596913666828));
#28131=CARTESIAN_POINT('Ctrl Pts',(-0.429803062482217,1.,1.88044229001778));
#28132=CARTESIAN_POINT('Ctrl Pts',(-0.427183828518743,1.,1.87486989291333));
#28133=CARTESIAN_POINT('Ctrl Pts',(-0.424678177290876,1.,1.8693780394412));
#28134=CARTESIAN_POINT('Ctrl Pts',(-0.422327307417885,1.,1.86408083333863));
#28135=CARTESIAN_POINT('Ctrl Pts',(-0.420157287975583,1.,1.8590328109667));
#28136=CARTESIAN_POINT('Ctrl Pts',(-0.418164129144045,1.,1.8541763285645));
#28137=CARTESIAN_POINT('Ctrl Pts',(-0.416300022039885,1.,1.84929312930314));
#28138=CARTESIAN_POINT('Ctrl Pts',(-0.414487438255542,1.,1.84405757074218));
#28139=CARTESIAN_POINT('Ctrl Pts',(-0.412633125322945,1.,1.8380895347617));
#28140=CARTESIAN_POINT('Ctrl Pts',(-0.410641256301276,1.,1.83100408895047));
#28141=CARTESIAN_POINT('Ctrl Pts',(-0.408428948106227,1.,1.82247022677562));
#28142=CARTESIAN_POINT('Ctrl Pts',(-0.405933518407175,1.,1.81223801812013));
#28143=CARTESIAN_POINT('Ctrl Pts',(-0.403107976163396,1.,1.80012077173238));
#28144=CARTESIAN_POINT('Ctrl Pts',(-0.399919403774155,1.,1.78598826343754));
#28145=CARTESIAN_POINT('Ctrl Pts',(-0.396346196110688,1.,1.76975560043442));
#28146=CARTESIAN_POINT('Ctrl Pts',(-0.392375812285395,1.,1.75137405310193));
#28147=CARTESIAN_POINT('Ctrl Pts',(-0.388877023502615,1.,1.73493170972829));
#28148=CARTESIAN_POINT('Ctrl Pts',(-0.386070790323281,1.,1.72162022244582));
#28149=CARTESIAN_POINT('Ctrl Pts',(-0.384119047314215,1.,1.71231062891398));
#28150=CARTESIAN_POINT('Ctrl Pts',(-0.383122945602004,1.,1.7075470150345));
#28151=CARTESIAN_POINT('',(-0.61342227326009,0.,2.11275013067528));
#28152=CARTESIAN_POINT('Origin',(-0.745574324794401,0.,2.0698113262342));
#28153=CARTESIAN_POINT('',(-0.745574324794401,1.,2.0698113262342));
#28154=CARTESIAN_POINT('',(-0.61342227326009,1.,2.11275013067528));
#28155=CARTESIAN_POINT('',(-0.745574324794401,0.,2.0698113262342));
#28156=CARTESIAN_POINT('Ctrl Pts',(-0.693717979106306,-1.,1.60662857109684));
#28157=CARTESIAN_POINT('Ctrl Pts',(-0.693717979106306,1.,1.60662857109684));
#28158=CARTESIAN_POINT('Ctrl Pts',(-0.695712097881194,-1.,1.61106790958151));
#28159=CARTESIAN_POINT('Ctrl Pts',(-0.695712097881194,1.,1.61106790958151));
#28160=CARTESIAN_POINT('Ctrl Pts',(-0.699605146405088,-1.,1.61974673472612));
#28161=CARTESIAN_POINT('Ctrl Pts',(-0.699605146405088,1.,1.61974673472612));
#28162=CARTESIAN_POINT('Ctrl Pts',(-0.705159151988319,-1.,1.63216541664676));
#28163=CARTESIAN_POINT('Ctrl Pts',(-0.705159151988319,1.,1.63216541664676));
#28164=CARTESIAN_POINT('Ctrl Pts',(-0.711993139355394,-1.,1.64752408832016));
#28165=CARTESIAN_POINT('Ctrl Pts',(-0.711993139355394,1.,1.64752408832016));
#28166=CARTESIAN_POINT('Ctrl Pts',(-0.719585433804282,-1.,1.6647288055568));
#28167=CARTESIAN_POINT('Ctrl Pts',(-0.719585433804282,1.,1.6647288055568));
#28168=CARTESIAN_POINT('Ctrl Pts',(-0.726235967997433,-1.,1.67996158455503));
#28169=CARTESIAN_POINT('Ctrl Pts',(-0.726235967997433,1.,1.67996158455503));
#28170=CARTESIAN_POINT('Ctrl Pts',(-0.731963238697195,-1.,1.69326921975743));
#28171=CARTESIAN_POINT('Ctrl Pts',(-0.731963238697195,1.,1.69326921975743));
#28172=CARTESIAN_POINT('Ctrl Pts',(-0.736799665724771,-1.,1.70473309006121));
#28173=CARTESIAN_POINT('Ctrl Pts',(-0.736799665724771,1.,1.70473309006121));
#28174=CARTESIAN_POINT('Ctrl Pts',(-0.740795162032088,-1.,1.71447789751927));
#28175=CARTESIAN_POINT('Ctrl Pts',(-0.740795162032088,1.,1.71447789751927));
#28176=CARTESIAN_POINT('Ctrl Pts',(-0.744021445433764,-1.,1.7226822991693));
#28177=CARTESIAN_POINT('Ctrl Pts',(-0.744021445433764,1.,1.7226822991693));
#28178=CARTESIAN_POINT('Ctrl Pts',(-0.746574710096436,-1.,1.72958533647399));
#28179=CARTESIAN_POINT('Ctrl Pts',(-0.746574710096436,1.,1.72958533647399));
#28180=CARTESIAN_POINT('Ctrl Pts',(-0.748582462954855,-1.,1.73550351679848));
#28181=CARTESIAN_POINT('Ctrl Pts',(-0.748582462954855,1.,1.73550351679848));
#28182=CARTESIAN_POINT('Ctrl Pts',(-0.75019343597954,-1.,1.74080458266705));
#28183=CARTESIAN_POINT('Ctrl Pts',(-0.75019343597954,1.,1.74080458266705));
#28184=CARTESIAN_POINT('Ctrl Pts',(-0.751555614163629,-1.,1.74585086852298));
#28185=CARTESIAN_POINT('Ctrl Pts',(-0.751555614163629,1.,1.74585086852298));
#28186=CARTESIAN_POINT('Ctrl Pts',(-0.752797683531377,-1.,1.75095139468809));
#28187=CARTESIAN_POINT('Ctrl Pts',(-0.752797683531377,1.,1.75095139468809));
#28188=CARTESIAN_POINT('Ctrl Pts',(-0.75400925402848,-1.,1.75631083600175));
#28189=CARTESIAN_POINT('Ctrl Pts',(-0.75400925402848,1.,1.75631083600175));
#28190=CARTESIAN_POINT('Ctrl Pts',(-0.755220979975262,-1.,1.7619781724032));
#28191=CARTESIAN_POINT('Ctrl Pts',(-0.755220979975262,1.,1.7619781724032));
#28192=CARTESIAN_POINT('Ctrl Pts',(-0.756421896028403,-1.,1.76789396003141));
#28193=CARTESIAN_POINT('Ctrl Pts',(-0.756421896028403,1.,1.76789396003141));
#28194=CARTESIAN_POINT('Ctrl Pts',(-0.757578264077238,-1.,1.77394167108342));
#28195=CARTESIAN_POINT('Ctrl Pts',(-0.757578264077238,1.,1.77394167108342));
#28196=CARTESIAN_POINT('Ctrl Pts',(-0.75865062667738,-1.,1.77999411220912));
#28197=CARTESIAN_POINT('Ctrl Pts',(-0.75865062667738,1.,1.77999411220912));
#28198=CARTESIAN_POINT('Ctrl Pts',(-0.759614401109868,-1.,1.78596964884526));
#28199=CARTESIAN_POINT('Ctrl Pts',(-0.759614401109868,1.,1.78596964884526));
#28200=CARTESIAN_POINT('Ctrl Pts',(-0.760469555880425,-1.,1.79185815610802));
#28201=CARTESIAN_POINT('Ctrl Pts',(-0.760469555880425,1.,1.79185815610802));
#28202=CARTESIAN_POINT('Ctrl Pts',(-0.761229695230359,-1.,1.79768986997735));
#28203=CARTESIAN_POINT('Ctrl Pts',(-0.761229695230359,1.,1.79768986997735));
#28204=CARTESIAN_POINT('Ctrl Pts',(-0.761915336443516,-1.,1.80351583877334));
#28205=CARTESIAN_POINT('Ctrl Pts',(-0.761915336443516,1.,1.80351583877334));
#28206=CARTESIAN_POINT('Ctrl Pts',(-0.762546129464036,-1.,1.80938551463989));
#28207=CARTESIAN_POINT('Ctrl Pts',(-0.762546129464036,1.,1.80938551463989));
#28208=CARTESIAN_POINT('Ctrl Pts',(-0.763132003836783,-1.,1.81532118405566));
#28209=CARTESIAN_POINT('Ctrl Pts',(-0.763132003836783,1.,1.81532118405566));
#28210=CARTESIAN_POINT('Ctrl Pts',(-0.763673465462854,-1.,1.82131873145297));
#28211=CARTESIAN_POINT('Ctrl Pts',(-0.763673465462854,1.,1.82131873145297));
#28212=CARTESIAN_POINT('Ctrl Pts',(-0.764165902606055,-1.,1.8273599120008));
#28213=CARTESIAN_POINT('Ctrl Pts',(-0.764165902606055,1.,1.8273599120008));
#28214=CARTESIAN_POINT('Ctrl Pts',(-0.764602549687845,-1.,1.8334207722714));
#28215=CARTESIAN_POINT('Ctrl Pts',(-0.764602549687845,1.,1.8334207722714));
#28216=CARTESIAN_POINT('Ctrl Pts',(-0.764978057881687,-1.,1.83948181064823));
#28217=CARTESIAN_POINT('Ctrl Pts',(-0.764978057881687,1.,1.83948181064823));
#28218=CARTESIAN_POINT('Ctrl Pts',(-0.765291664861971,-1.,1.8455369887591));
#28219=CARTESIAN_POINT('Ctrl Pts',(-0.765291664861971,1.,1.8455369887591));
#28220=CARTESIAN_POINT('Ctrl Pts',(-0.765545710619023,-1.,1.85158945130054));
#28221=CARTESIAN_POINT('Ctrl Pts',(-0.765545710619023,1.,1.85158945130054));
#28222=CARTESIAN_POINT('Ctrl Pts',(-0.765744212909305,-1.,1.85764741390391));
#28223=CARTESIAN_POINT('Ctrl Pts',(-0.765744212909305,1.,1.85764741390391));
#28224=CARTESIAN_POINT('Ctrl Pts',(-0.765891519092557,-1.,1.86372027063314));
#28225=CARTESIAN_POINT('Ctrl Pts',(-0.765891519092557,1.,1.86372027063314));
#28226=CARTESIAN_POINT('Ctrl Pts',(-0.765990708546111,-1.,1.86981398314345));
#28227=CARTESIAN_POINT('Ctrl Pts',(-0.765990708546111,1.,1.86981398314345));
#28228=CARTESIAN_POINT('Ctrl Pts',(-0.766042837036759,-1.,1.87592888967886));
#28229=CARTESIAN_POINT('Ctrl Pts',(-0.766042837036759,1.,1.87592888967886));
#28230=CARTESIAN_POINT('Ctrl Pts',(-0.766047794851869,-1.,1.88206215302561));
#28231=CARTESIAN_POINT('Ctrl Pts',(-0.766047794851869,1.,1.88206215302561));
#28232=CARTESIAN_POINT('Ctrl Pts',(-0.76600483706209,-1.,1.88820926433409));
#28233=CARTESIAN_POINT('Ctrl Pts',(-0.76600483706209,1.,1.88820926433409));
#28234=CARTESIAN_POINT('Ctrl Pts',(-0.765913193856979,-1.,1.89436577771389));
#28235=CARTESIAN_POINT('Ctrl Pts',(-0.765913193856979,1.,1.89436577771389));
#28236=CARTESIAN_POINT('Ctrl Pts',(-0.765772772593395,-1.,1.90052930393599));
#28237=CARTESIAN_POINT('Ctrl Pts',(-0.765772772593395,1.,1.90052930393599));
#28238=CARTESIAN_POINT('Ctrl Pts',(-0.765584196937936,-1.,1.90669961402362));
#28239=CARTESIAN_POINT('Ctrl Pts',(-0.765584196937936,1.,1.90669961402362));
#28240=CARTESIAN_POINT('Ctrl Pts',(-0.765348465884739,-1.,1.91287765805174));
#28241=CARTESIAN_POINT('Ctrl Pts',(-0.765348465884739,1.,1.91287765805174));
#28242=CARTESIAN_POINT('Ctrl Pts',(-0.765066729667095,-1.,1.91906491634197));
#28243=CARTESIAN_POINT('Ctrl Pts',(-0.765066729667095,1.,1.91906491634197));
#28244=CARTESIAN_POINT('Ctrl Pts',(-0.764740025488189,-1.,1.92526263537041));
#28245=CARTESIAN_POINT('Ctrl Pts',(-0.764740025488189,1.,1.92526263537041));
#28246=CARTESIAN_POINT('Ctrl Pts',(-0.764369010673889,-1.,1.93147105496367));
#28247=CARTESIAN_POINT('Ctrl Pts',(-0.764369010673889,1.,1.93147105496367));
#28248=CARTESIAN_POINT('Ctrl Pts',(-0.763954049121393,-1.,1.93768964875867));
#28249=CARTESIAN_POINT('Ctrl Pts',(-0.763954049121393,1.,1.93768964875867));
#28250=CARTESIAN_POINT('Ctrl Pts',(-0.76349533353858,-1.,1.94391746617626));
#28251=CARTESIAN_POINT('Ctrl Pts',(-0.76349533353858,1.,1.94391746617626));
#28252=CARTESIAN_POINT('Ctrl Pts',(-0.762992990878774,-1.,1.95015342590025));
#28253=CARTESIAN_POINT('Ctrl Pts',(-0.762992990878774,1.,1.95015342590025));
#28254=CARTESIAN_POINT('Ctrl Pts',(-0.762447203806263,-1.,1.95639665309893));
#28255=CARTESIAN_POINT('Ctrl Pts',(-0.762447203806263,1.,1.95639665309893));
#28256=CARTESIAN_POINT('Ctrl Pts',(-0.761858300014575,-1.,1.96264672744229));
#28257=CARTESIAN_POINT('Ctrl Pts',(-0.761858300014575,1.,1.96264672744229));
#28258=CARTESIAN_POINT('Ctrl Pts',(-0.761226690483986,-1.,1.96890351582545));
#28259=CARTESIAN_POINT('Ctrl Pts',(-0.761226690483986,1.,1.96890351582545));
#28260=CARTESIAN_POINT('Ctrl Pts',(-0.760552825409855,-1.,1.97516705321521));
#28261=CARTESIAN_POINT('Ctrl Pts',(-0.760552825409855,1.,1.97516705321521));
#28262=CARTESIAN_POINT('Ctrl Pts',(-0.759837147452135,-1.,1.98143741418156));
#28263=CARTESIAN_POINT('Ctrl Pts',(-0.759837147452135,1.,1.98143741418156));
#28264=CARTESIAN_POINT('Ctrl Pts',(-0.759080037802243,-1.,1.98771456680806));
#28265=CARTESIAN_POINT('Ctrl Pts',(-0.759080037802243,1.,1.98771456680806));
#28266=CARTESIAN_POINT('Ctrl Pts',(-0.758281796766377,-1.,1.9939983109871));
#28267=CARTESIAN_POINT('Ctrl Pts',(-0.758281796766377,1.,1.9939983109871));
#28268=CARTESIAN_POINT('Ctrl Pts',(-0.757442676862341,-1.,2.00028834739072));
#28269=CARTESIAN_POINT('Ctrl Pts',(-0.757442676862341,1.,2.00028834739072));
#28270=CARTESIAN_POINT('Ctrl Pts',(-0.756562904646496,-1.,2.00658431587682));
#28271=CARTESIAN_POINT('Ctrl Pts',(-0.756562904646496,1.,2.00658431587682));
#28272=CARTESIAN_POINT('Ctrl Pts',(-0.7556427049581,-1.,2.01288584328149));
#28273=CARTESIAN_POINT('Ctrl Pts',(-0.7556427049581,1.,2.01288584328149));
#28274=CARTESIAN_POINT('Ctrl Pts',(-0.75468233072352,-1.,2.01919259406003));
#28275=CARTESIAN_POINT('Ctrl Pts',(-0.75468233072352,1.,2.01919259406003));
#28276=CARTESIAN_POINT('Ctrl Pts',(-0.753682061113766,-1.,2.02550428623587));
#28277=CARTESIAN_POINT('Ctrl Pts',(-0.753682061113766,1.,2.02550428623587));
#28278=CARTESIAN_POINT('Ctrl Pts',(-0.752642180488104,-1.,2.03182068456467));
#28279=CARTESIAN_POINT('Ctrl Pts',(-0.752642180488104,1.,2.03182068456467));
#28280=CARTESIAN_POINT('Ctrl Pts',(-0.751562963361384,-1.,2.03814160092173));
#28281=CARTESIAN_POINT('Ctrl Pts',(-0.751562963361384,1.,2.03814160092173));
#28282=CARTESIAN_POINT('Ctrl Pts',(-0.750444657874758,-1.,2.04446689147754));
#28283=CARTESIAN_POINT('Ctrl Pts',(-0.750444657874758,1.,2.04446689147754));
#28284=CARTESIAN_POINT('Ctrl Pts',(-0.749287468663053,-1.,2.05079645591606));
#28285=CARTESIAN_POINT('Ctrl Pts',(-0.749287468663053,1.,2.05079645591606));
#28286=CARTESIAN_POINT('Ctrl Pts',(-0.748091554181101,-1.,2.05713023030263));
#28287=CARTESIAN_POINT('Ctrl Pts',(-0.748091554181101,1.,2.05713023030263));
#28288=CARTESIAN_POINT('Ctrl Pts',(-0.747103932785504,-1.,2.06220058927162));
#28289=CARTESIAN_POINT('Ctrl Pts',(-0.747103932785504,1.,2.06220058927162));
#28290=CARTESIAN_POINT('Ctrl Pts',(-0.746345871542696,-1.,2.06600523016401));
#28291=CARTESIAN_POINT('Ctrl Pts',(-0.746345871542696,1.,2.06600523016401));
#28292=CARTESIAN_POINT('Ctrl Pts',(-0.74583279137781,-1.,2.06854248895575));
#28293=CARTESIAN_POINT('Ctrl Pts',(-0.74583279137781,1.,2.06854248895575));
#28294=CARTESIAN_POINT('Ctrl Pts',(-0.745574324794401,-1.,2.0698113262342));
#28295=CARTESIAN_POINT('Ctrl Pts',(-0.745574324794401,1.,2.0698113262342));
#28296=CARTESIAN_POINT('',(-0.693717979106306,1.,1.60662857109684));
#28297=CARTESIAN_POINT('Ctrl Pts',(-0.693717979106306,1.,1.60662857109684));
#28298=CARTESIAN_POINT('Ctrl Pts',(-0.695712097881194,1.,1.61106790958151));
#28299=CARTESIAN_POINT('Ctrl Pts',(-0.699605146405088,1.,1.61974673472612));
#28300=CARTESIAN_POINT('Ctrl Pts',(-0.705159151988319,1.,1.63216541664676));
#28301=CARTESIAN_POINT('Ctrl Pts',(-0.711993139355394,1.,1.64752408832016));
#28302=CARTESIAN_POINT('Ctrl Pts',(-0.719585433804282,1.,1.6647288055568));
#28303=CARTESIAN_POINT('Ctrl Pts',(-0.726235967997433,1.,1.67996158455503));
#28304=CARTESIAN_POINT('Ctrl Pts',(-0.731963238697195,1.,1.69326921975743));
#28305=CARTESIAN_POINT('Ctrl Pts',(-0.736799665724771,1.,1.70473309006121));
#28306=CARTESIAN_POINT('Ctrl Pts',(-0.740795162032088,1.,1.71447789751927));
#28307=CARTESIAN_POINT('Ctrl Pts',(-0.744021445433764,1.,1.7226822991693));
#28308=CARTESIAN_POINT('Ctrl Pts',(-0.746574710096436,1.,1.72958533647399));
#28309=CARTESIAN_POINT('Ctrl Pts',(-0.748582462954855,1.,1.73550351679848));
#28310=CARTESIAN_POINT('Ctrl Pts',(-0.75019343597954,1.,1.74080458266705));
#28311=CARTESIAN_POINT('Ctrl Pts',(-0.751555614163629,1.,1.74585086852298));
#28312=CARTESIAN_POINT('Ctrl Pts',(-0.752797683531377,1.,1.75095139468809));
#28313=CARTESIAN_POINT('Ctrl Pts',(-0.75400925402848,1.,1.75631083600175));
#28314=CARTESIAN_POINT('Ctrl Pts',(-0.755220979975262,1.,1.7619781724032));
#28315=CARTESIAN_POINT('Ctrl Pts',(-0.756421896028403,1.,1.76789396003141));
#28316=CARTESIAN_POINT('Ctrl Pts',(-0.757578264077238,1.,1.77394167108342));
#28317=CARTESIAN_POINT('Ctrl Pts',(-0.75865062667738,1.,1.77999411220912));
#28318=CARTESIAN_POINT('Ctrl Pts',(-0.759614401109868,1.,1.78596964884526));
#28319=CARTESIAN_POINT('Ctrl Pts',(-0.760469555880425,1.,1.79185815610802));
#28320=CARTESIAN_POINT('Ctrl Pts',(-0.761229695230359,1.,1.79768986997735));
#28321=CARTESIAN_POINT('Ctrl Pts',(-0.761915336443516,1.,1.80351583877334));
#28322=CARTESIAN_POINT('Ctrl Pts',(-0.762546129464036,1.,1.80938551463989));
#28323=CARTESIAN_POINT('Ctrl Pts',(-0.763132003836783,1.,1.81532118405566));
#28324=CARTESIAN_POINT('Ctrl Pts',(-0.763673465462854,1.,1.82131873145297));
#28325=CARTESIAN_POINT('Ctrl Pts',(-0.764165902606055,1.,1.8273599120008));
#28326=CARTESIAN_POINT('Ctrl Pts',(-0.764602549687845,1.,1.8334207722714));
#28327=CARTESIAN_POINT('Ctrl Pts',(-0.764978057881687,1.,1.83948181064823));
#28328=CARTESIAN_POINT('Ctrl Pts',(-0.765291664861971,1.,1.8455369887591));
#28329=CARTESIAN_POINT('Ctrl Pts',(-0.765545710619023,1.,1.85158945130054));
#28330=CARTESIAN_POINT('Ctrl Pts',(-0.765744212909305,1.,1.85764741390391));
#28331=CARTESIAN_POINT('Ctrl Pts',(-0.765891519092557,1.,1.86372027063314));
#28332=CARTESIAN_POINT('Ctrl Pts',(-0.765990708546111,1.,1.86981398314345));
#28333=CARTESIAN_POINT('Ctrl Pts',(-0.766042837036759,1.,1.87592888967886));
#28334=CARTESIAN_POINT('Ctrl Pts',(-0.766047794851869,1.,1.88206215302561));
#28335=CARTESIAN_POINT('Ctrl Pts',(-0.76600483706209,1.,1.88820926433409));
#28336=CARTESIAN_POINT('Ctrl Pts',(-0.765913193856979,1.,1.89436577771389));
#28337=CARTESIAN_POINT('Ctrl Pts',(-0.765772772593395,1.,1.90052930393599));
#28338=CARTESIAN_POINT('Ctrl Pts',(-0.765584196937936,1.,1.90669961402362));
#28339=CARTESIAN_POINT('Ctrl Pts',(-0.765348465884739,1.,1.91287765805174));
#28340=CARTESIAN_POINT('Ctrl Pts',(-0.765066729667095,1.,1.91906491634197));
#28341=CARTESIAN_POINT('Ctrl Pts',(-0.764740025488189,1.,1.92526263537041));
#28342=CARTESIAN_POINT('Ctrl Pts',(-0.764369010673889,1.,1.93147105496367));
#28343=CARTESIAN_POINT('Ctrl Pts',(-0.763954049121393,1.,1.93768964875867));
#28344=CARTESIAN_POINT('Ctrl Pts',(-0.76349533353858,1.,1.94391746617626));
#28345=CARTESIAN_POINT('Ctrl Pts',(-0.762992990878774,1.,1.95015342590025));
#28346=CARTESIAN_POINT('Ctrl Pts',(-0.762447203806263,1.,1.95639665309893));
#28347=CARTESIAN_POINT('Ctrl Pts',(-0.761858300014575,1.,1.96264672744229));
#28348=CARTESIAN_POINT('Ctrl Pts',(-0.761226690483986,1.,1.96890351582545));
#28349=CARTESIAN_POINT('Ctrl Pts',(-0.760552825409855,1.,1.97516705321521));
#28350=CARTESIAN_POINT('Ctrl Pts',(-0.759837147452135,1.,1.98143741418156));
#28351=CARTESIAN_POINT('Ctrl Pts',(-0.759080037802243,1.,1.98771456680806));
#28352=CARTESIAN_POINT('Ctrl Pts',(-0.758281796766377,1.,1.9939983109871));
#28353=CARTESIAN_POINT('Ctrl Pts',(-0.757442676862341,1.,2.00028834739072));
#28354=CARTESIAN_POINT('Ctrl Pts',(-0.756562904646496,1.,2.00658431587682));
#28355=CARTESIAN_POINT('Ctrl Pts',(-0.7556427049581,1.,2.01288584328149));
#28356=CARTESIAN_POINT('Ctrl Pts',(-0.75468233072352,1.,2.01919259406003));
#28357=CARTESIAN_POINT('Ctrl Pts',(-0.753682061113766,1.,2.02550428623587));
#28358=CARTESIAN_POINT('Ctrl Pts',(-0.752642180488104,1.,2.03182068456467));
#28359=CARTESIAN_POINT('Ctrl Pts',(-0.751562963361384,1.,2.03814160092173));
#28360=CARTESIAN_POINT('Ctrl Pts',(-0.750444657874758,1.,2.04446689147754));
#28361=CARTESIAN_POINT('Ctrl Pts',(-0.749287468663053,1.,2.05079645591606));
#28362=CARTESIAN_POINT('Ctrl Pts',(-0.748091554181101,1.,2.05713023030263));
#28363=CARTESIAN_POINT('Ctrl Pts',(-0.747103932785504,1.,2.06220058927162));
#28364=CARTESIAN_POINT('Ctrl Pts',(-0.746345871542696,1.,2.06600523016401));
#28365=CARTESIAN_POINT('Ctrl Pts',(-0.74583279137781,1.,2.06854248895575));
#28366=CARTESIAN_POINT('Ctrl Pts',(-0.745574324794401,1.,2.0698113262342));
#28367=CARTESIAN_POINT('',(-0.693717979106306,0.,1.60662857109684));
#28368=CARTESIAN_POINT('Origin',(0.,0.,0.));
#28369=CARTESIAN_POINT('',(-0.892032620296855,1.,1.5055822144029));
#28370=CARTESIAN_POINT('Origin',(0.,1.,0.));
#28371=CARTESIAN_POINT('',(-0.892032620296855,0.,1.5055822144029));
#28372=CARTESIAN_POINT('Ctrl Pts',(-1.23627494547115,-1.,1.81978687191668));
#28373=CARTESIAN_POINT('Ctrl Pts',(-1.23627494547115,1.,1.81978687191668));
#28374=CARTESIAN_POINT('Ctrl Pts',(-1.23509651170476,-1.,1.81925017193666));
#28375=CARTESIAN_POINT('Ctrl Pts',(-1.23509651170476,1.,1.81925017193666));
#28376=CARTESIAN_POINT('Ctrl Pts',(-1.2327422452705,-1.,1.81817389921279));
#28377=CARTESIAN_POINT('Ctrl Pts',(-1.2327422452705,1.,1.81817389921279));
#28378=CARTESIAN_POINT('Ctrl Pts',(-1.2292186489137,-1.,1.8165508718364));
#28379=CARTESIAN_POINT('Ctrl Pts',(-1.2292186489137,1.,1.8165508718364));
#28380=CARTESIAN_POINT('Ctrl Pts',(-1.2245361330495,-1.,1.81436959210434));
#28381=CARTESIAN_POINT('Ctrl Pts',(-1.2245361330495,1.,1.81436959210434));
#28382=CARTESIAN_POINT('Ctrl Pts',(-1.21870906103557,-1.,1.81161420806656));
#28383=CARTESIAN_POINT('Ctrl Pts',(-1.21870906103557,1.,1.81161420806656));
#28384=CARTESIAN_POINT('Ctrl Pts',(-1.21290815708314,-1.,1.80882996917129));
#28385=CARTESIAN_POINT('Ctrl Pts',(-1.21290815708314,1.,1.80882996917129));
#28386=CARTESIAN_POINT('Ctrl Pts',(-1.20713356605475,-1.,1.80601678480707));
#28387=CARTESIAN_POINT('Ctrl Pts',(-1.20713356605475,1.,1.80601678480707));
#28388=CARTESIAN_POINT('Ctrl Pts',(-1.20138548938974,-1.,1.80317454838603));
#28389=CARTESIAN_POINT('Ctrl Pts',(-1.20138548938974,1.,1.80317454838603));
#28390=CARTESIAN_POINT('Ctrl Pts',(-1.19566418930242,-1.,1.80030314369879));
#28391=CARTESIAN_POINT('Ctrl Pts',(-1.19566418930242,1.,1.80030314369879));
#28392=CARTESIAN_POINT('Ctrl Pts',(-1.18996997934445,-1.,1.79740245923478));
#28393=CARTESIAN_POINT('Ctrl Pts',(-1.18996997934445,1.,1.79740245923478));
#28394=CARTESIAN_POINT('Ctrl Pts',(-1.18430321697432,-1.,1.79447240321515));
#28395=CARTESIAN_POINT('Ctrl Pts',(-1.18430321697432,1.,1.79447240321515));
#28396=CARTESIAN_POINT('Ctrl Pts',(-1.17866429440809,-1.,1.79151291552689));
#28397=CARTESIAN_POINT('Ctrl Pts',(-1.17866429440809,1.,1.79151291552689));
#28398=CARTESIAN_POINT('Ctrl Pts',(-1.17305363177328,-1.,1.78852398877616));
#28399=CARTESIAN_POINT('Ctrl Pts',(-1.17305363177328,1.,1.78852398877616));
#28400=CARTESIAN_POINT('Ctrl Pts',(-1.16747166312303,-1.,1.78550566040443));
#28401=CARTESIAN_POINT('Ctrl Pts',(-1.16747166312303,1.,1.78550566040443));
#28402=CARTESIAN_POINT('Ctrl Pts',(-1.16191881298499,-1.,1.78245795881009));
#28403=CARTESIAN_POINT('Ctrl Pts',(-1.16191881298499,1.,1.78245795881009));
#28404=CARTESIAN_POINT('Ctrl Pts',(-1.15639547194698,-1.,1.77938085564275));
#28405=CARTESIAN_POINT('Ctrl Pts',(-1.15639547194698,1.,1.77938085564275));
#28406=CARTESIAN_POINT('Ctrl Pts',(-1.15090197841515,-1.,1.7762742255701));
#28407=CARTESIAN_POINT('Ctrl Pts',(-1.15090197841515,1.,1.7762742255701));
#28408=CARTESIAN_POINT('Ctrl Pts',(-1.1454385822692,-1.,1.77313777896194));
#28409=CARTESIAN_POINT('Ctrl Pts',(-1.1454385822692,1.,1.77313777896194));
#28410=CARTESIAN_POINT('Ctrl Pts',(-1.14000548336975,-1.,1.76997111386769));
#28411=CARTESIAN_POINT('Ctrl Pts',(-1.14000548336975,1.,1.76997111386769));
#28412=CARTESIAN_POINT('Ctrl Pts',(-1.1346029180462,-1.,1.76677384551862));
#28413=CARTESIAN_POINT('Ctrl Pts',(-1.1346029180462,1.,1.76677384551862));
#28414=CARTESIAN_POINT('Ctrl Pts',(-1.12923123555075,-1.,1.7635457196617));
#28415=CARTESIAN_POINT('Ctrl Pts',(-1.12923123555075,1.,1.7635457196617));
#28416=CARTESIAN_POINT('Ctrl Pts',(-1.12389096855086,-1.,1.76028671825096));
#28417=CARTESIAN_POINT('Ctrl Pts',(-1.12389096855086,1.,1.76028671825096));
#28418=CARTESIAN_POINT('Ctrl Pts',(-1.11858293216763,-1.,1.75699720772105));
#28419=CARTESIAN_POINT('Ctrl Pts',(-1.11858293216763,1.,1.75699720772105));
#28420=CARTESIAN_POINT('Ctrl Pts',(-1.11330807582551,-1.,1.7536777209463));
#28421=CARTESIAN_POINT('Ctrl Pts',(-1.11330807582551,1.,1.7536777209463));
#28422=CARTESIAN_POINT('Ctrl Pts',(-1.10806728183007,-1.,1.7503286607592));
#28423=CARTESIAN_POINT('Ctrl Pts',(-1.10806728183007,1.,1.7503286607592));
#28424=CARTESIAN_POINT('Ctrl Pts',(-1.10286118991143,-1.,1.74695004214923));
#28425=CARTESIAN_POINT('Ctrl Pts',(-1.10286118991143,1.,1.74695004214923));
#28426=CARTESIAN_POINT('Ctrl Pts',(-1.09768999241225,-1.,1.74354119236208));
#28427=CARTESIAN_POINT('Ctrl Pts',(-1.09768999241225,1.,1.74354119236208));
#28428=CARTESIAN_POINT('Ctrl Pts',(-1.09255329056493,-1.,1.74010053962247));
#28429=CARTESIAN_POINT('Ctrl Pts',(-1.09255329056493,1.,1.74010053962247));
#28430=CARTESIAN_POINT('Ctrl Pts',(-1.08745056285427,-1.,1.73662628326091));
#28431=CARTESIAN_POINT('Ctrl Pts',(-1.08745056285427,1.,1.73662628326091));
#28432=CARTESIAN_POINT('Ctrl Pts',(-1.08238162784749,-1.,1.73311705663407));
#28433=CARTESIAN_POINT('Ctrl Pts',(-1.08238162784749,1.,1.73311705663407));
#28434=CARTESIAN_POINT('Ctrl Pts',(-1.0773470373727,-1.,1.72957248977424));
#28435=CARTESIAN_POINT('Ctrl Pts',(-1.0773470373727,1.,1.72957248977424));
#28436=CARTESIAN_POINT('Ctrl Pts',(-1.07234866990252,-1.,1.72599406198488));
#28437=CARTESIAN_POINT('Ctrl Pts',(-1.07234866990252,1.,1.72599406198488));
#28438=CARTESIAN_POINT('Ctrl Pts',(-1.06738966975462,-1.,1.72238500928453));
#28439=CARTESIAN_POINT('Ctrl Pts',(-1.06738966975462,1.,1.72238500928453));
#28440=CARTESIAN_POINT('Ctrl Pts',(-1.06247324680647,-1.,1.71874858456904));
#28441=CARTESIAN_POINT('Ctrl Pts',(-1.06247324680647,1.,1.71874858456904));
#28442=CARTESIAN_POINT('Ctrl Pts',(-1.05760163192479,-1.,1.7150865442702));
#28443=CARTESIAN_POINT('Ctrl Pts',(-1.05760163192479,1.,1.7150865442702));
#28444=CARTESIAN_POINT('Ctrl Pts',(-1.05277517202855,-1.,1.71139783543989));
#28445=CARTESIAN_POINT('Ctrl Pts',(-1.05277517202855,1.,1.71139783543989));
#28446=CARTESIAN_POINT('Ctrl Pts',(-1.04799085404995,-1.,1.70767646263649));
#28447=CARTESIAN_POINT('Ctrl Pts',(-1.04799085404995,1.,1.70767646263649));
#28448=CARTESIAN_POINT('Ctrl Pts',(-1.04324363334554,-1.,1.70391338707982));
#28449=CARTESIAN_POINT('Ctrl Pts',(-1.04324363334554,1.,1.70391338707982));
#28450=CARTESIAN_POINT('Ctrl Pts',(-1.03852922490789,-1.,1.70010052930962));
#28451=CARTESIAN_POINT('Ctrl Pts',(-1.03852922490789,1.,1.70010052930962));
#28452=CARTESIAN_POINT('Ctrl Pts',(-1.03384646003588,-1.,1.69623414782771));
#28453=CARTESIAN_POINT('Ctrl Pts',(-1.03384646003588,1.,1.69623414782771));
#28454=CARTESIAN_POINT('Ctrl Pts',(-1.02919977579147,-1.,1.69231840863458));
#28455=CARTESIAN_POINT('Ctrl Pts',(-1.02919977579147,1.,1.69231840863458));
#28456=CARTESIAN_POINT('Ctrl Pts',(-1.02460180535255,-1.,1.68836910178447));
#28457=CARTESIAN_POINT('Ctrl Pts',(-1.02460180535255,1.,1.68836910178447));
#28458=CARTESIAN_POINT('Ctrl Pts',(-1.02006795074201,-1.,1.68440578021706));
#28459=CARTESIAN_POINT('Ctrl Pts',(-1.02006795074201,1.,1.68440578021706));
#28460=CARTESIAN_POINT('Ctrl Pts',(-1.01561026162773,-1.,1.68044289894798));
#28461=CARTESIAN_POINT('Ctrl Pts',(-1.01561026162773,1.,1.68044289894798));
#28462=CARTESIAN_POINT('Ctrl Pts',(-1.01123236493511,-1.,1.67648246776464));
#28463=CARTESIAN_POINT('Ctrl Pts',(-1.01123236493511,1.,1.67648246776464));
#28464=CARTESIAN_POINT('Ctrl Pts',(-1.00692206696414,-1.,1.67250335383293));
#28465=CARTESIAN_POINT('Ctrl Pts',(-1.00692206696414,1.,1.67250335383293));
#28466=CARTESIAN_POINT('Ctrl Pts',(-1.00265091003727,-1.,1.66846059277303));
#28467=CARTESIAN_POINT('Ctrl Pts',(-1.00265091003727,1.,1.66846059277303));
#28468=CARTESIAN_POINT('Ctrl Pts',(-0.998389654952758,-1.,1.66430758030376));
#28469=CARTESIAN_POINT('Ctrl Pts',(-0.998389654952758,1.,1.66430758030376));
#28470=CARTESIAN_POINT('Ctrl Pts',(-0.994121836661306,-1.,1.66001553809947));
#28471=CARTESIAN_POINT('Ctrl Pts',(-0.994121836661306,1.,1.66001553809947));
#28472=CARTESIAN_POINT('Ctrl Pts',(-0.989855627854165,-1.,1.65559044289699));
#28473=CARTESIAN_POINT('Ctrl Pts',(-0.989855627854165,1.,1.65559044289699));
#28474=CARTESIAN_POINT('Ctrl Pts',(-0.985642622920821,-1.,1.65110016612638));
#28475=CARTESIAN_POINT('Ctrl Pts',(-0.985642622920821,1.,1.65110016612638));
#28476=CARTESIAN_POINT('Ctrl Pts',(-0.981562530939489,-1.,1.64665139190656));
#28477=CARTESIAN_POINT('Ctrl Pts',(-0.981562530939489,1.,1.64665139190656));
#28478=CARTESIAN_POINT('Ctrl Pts',(-0.977689794119416,-1.,1.64233990826687));
#28479=CARTESIAN_POINT('Ctrl Pts',(-0.977689794119416,1.,1.64233990826687));
#28480=CARTESIAN_POINT('Ctrl Pts',(-0.974066058287418,-1.,1.63820952658144));
#28481=CARTESIAN_POINT('Ctrl Pts',(-0.974066058287418,1.,1.63820952658144));
#28482=CARTESIAN_POINT('Ctrl Pts',(-0.970669715997509,-1.,1.63420665729798));
#28483=CARTESIAN_POINT('Ctrl Pts',(-0.970669715997509,1.,1.63420665729798));
#28484=CARTESIAN_POINT('Ctrl Pts',(-0.967387853230345,-1.,1.63013849959461));
#28485=CARTESIAN_POINT('Ctrl Pts',(-0.967387853230345,1.,1.63013849959461));
#28486=CARTESIAN_POINT('Ctrl Pts',(-0.964046107040536,-1.,1.62571930670187));
#28487=CARTESIAN_POINT('Ctrl Pts',(-0.964046107040536,1.,1.62571930670187));
#28488=CARTESIAN_POINT('Ctrl Pts',(-0.960438326101729,-1.,1.62061638140221));
#28489=CARTESIAN_POINT('Ctrl Pts',(-0.960438326101729,1.,1.62061638140221));
#28490=CARTESIAN_POINT('Ctrl Pts',(-0.956354422920671,-1.,1.61449324337085));
#28491=CARTESIAN_POINT('Ctrl Pts',(-0.956354422920671,1.,1.61449324337085));
#28492=CARTESIAN_POINT('Ctrl Pts',(-0.951613284356035,-1.,1.60706069896936));
#28493=CARTESIAN_POINT('Ctrl Pts',(-0.951613284356035,1.,1.60706069896936));
#28494=CARTESIAN_POINT('Ctrl Pts',(-0.946078063315257,-1.,1.59810042043673));
#28495=CARTESIAN_POINT('Ctrl Pts',(-0.946078063315257,1.,1.59810042043673));
#28496=CARTESIAN_POINT('Ctrl Pts',(-0.939646377893399,-1.,1.58744937487176));
#28497=CARTESIAN_POINT('Ctrl Pts',(-0.939646377893399,1.,1.58744937487176));
#28498=CARTESIAN_POINT('Ctrl Pts',(-0.932246680108685,-1.,1.57499388382243));
#28499=CARTESIAN_POINT('Ctrl Pts',(-0.932246680108685,1.,1.57499388382243));
#28500=CARTESIAN_POINT('Ctrl Pts',(-0.923832188944341,-1.,1.56065988578893));
#28501=CARTESIAN_POINT('Ctrl Pts',(-0.923832188944341,1.,1.56065988578893));
#28502=CARTESIAN_POINT('Ctrl Pts',(-0.914375919026456,-1.,1.54440491149498));
#28503=CARTESIAN_POINT('Ctrl Pts',(-0.914375919026456,1.,1.54440491149498));
#28504=CARTESIAN_POINT('Ctrl Pts',(-0.905967409625651,-1.,1.52984849887993));
#28505=CARTESIAN_POINT('Ctrl Pts',(-0.905967409625651,1.,1.52984849887993));
#28506=CARTESIAN_POINT('Ctrl Pts',(-0.899185047483511,-1.,1.51805569590094));
#28507=CARTESIAN_POINT('Ctrl Pts',(-0.899185047483511,1.,1.51805569590094));
#28508=CARTESIAN_POINT('Ctrl Pts',(-0.894452006964543,-1.,1.50980486806688));
#28509=CARTESIAN_POINT('Ctrl Pts',(-0.894452006964543,1.,1.50980486806688));
#28510=CARTESIAN_POINT('Ctrl Pts',(-0.892032620296855,-1.,1.5055822144029));
#28511=CARTESIAN_POINT('Ctrl Pts',(-0.892032620296855,1.,1.5055822144029));
#28512=CARTESIAN_POINT('',(-1.23627494547115,1.,1.81978687191668));
#28513=CARTESIAN_POINT('Ctrl Pts',(-1.23627494547115,1.,1.81978687191668));
#28514=CARTESIAN_POINT('Ctrl Pts',(-1.23509651170476,1.,1.81925017193666));
#28515=CARTESIAN_POINT('Ctrl Pts',(-1.2327422452705,1.,1.81817389921279));
#28516=CARTESIAN_POINT('Ctrl Pts',(-1.2292186489137,1.,1.8165508718364));
#28517=CARTESIAN_POINT('Ctrl Pts',(-1.2245361330495,1.,1.81436959210434));
#28518=CARTESIAN_POINT('Ctrl Pts',(-1.21870906103557,1.,1.81161420806656));
#28519=CARTESIAN_POINT('Ctrl Pts',(-1.21290815708314,1.,1.80882996917129));
#28520=CARTESIAN_POINT('Ctrl Pts',(-1.20713356605475,1.,1.80601678480707));
#28521=CARTESIAN_POINT('Ctrl Pts',(-1.20138548938974,1.,1.80317454838603));
#28522=CARTESIAN_POINT('Ctrl Pts',(-1.19566418930242,1.,1.80030314369879));
#28523=CARTESIAN_POINT('Ctrl Pts',(-1.18996997934445,1.,1.79740245923478));
#28524=CARTESIAN_POINT('Ctrl Pts',(-1.18430321697432,1.,1.79447240321515));
#28525=CARTESIAN_POINT('Ctrl Pts',(-1.17866429440809,1.,1.79151291552689));
#28526=CARTESIAN_POINT('Ctrl Pts',(-1.17305363177328,1.,1.78852398877616));
#28527=CARTESIAN_POINT('Ctrl Pts',(-1.16747166312303,1.,1.78550566040443));
#28528=CARTESIAN_POINT('Ctrl Pts',(-1.16191881298499,1.,1.78245795881009));
#28529=CARTESIAN_POINT('Ctrl Pts',(-1.15639547194698,1.,1.77938085564275));
#28530=CARTESIAN_POINT('Ctrl Pts',(-1.15090197841515,1.,1.7762742255701));
#28531=CARTESIAN_POINT('Ctrl Pts',(-1.1454385822692,1.,1.77313777896194));
#28532=CARTESIAN_POINT('Ctrl Pts',(-1.14000548336975,1.,1.76997111386769));
#28533=CARTESIAN_POINT('Ctrl Pts',(-1.1346029180462,1.,1.76677384551862));
#28534=CARTESIAN_POINT('Ctrl Pts',(-1.12923123555075,1.,1.7635457196617));
#28535=CARTESIAN_POINT('Ctrl Pts',(-1.12389096855086,1.,1.76028671825096));
#28536=CARTESIAN_POINT('Ctrl Pts',(-1.11858293216763,1.,1.75699720772105));
#28537=CARTESIAN_POINT('Ctrl Pts',(-1.11330807582551,1.,1.7536777209463));
#28538=CARTESIAN_POINT('Ctrl Pts',(-1.10806728183007,1.,1.7503286607592));
#28539=CARTESIAN_POINT('Ctrl Pts',(-1.10286118991143,1.,1.74695004214923));
#28540=CARTESIAN_POINT('Ctrl Pts',(-1.09768999241225,1.,1.74354119236208));
#28541=CARTESIAN_POINT('Ctrl Pts',(-1.09255329056493,1.,1.74010053962247));
#28542=CARTESIAN_POINT('Ctrl Pts',(-1.08745056285427,1.,1.73662628326091));
#28543=CARTESIAN_POINT('Ctrl Pts',(-1.08238162784749,1.,1.73311705663407));
#28544=CARTESIAN_POINT('Ctrl Pts',(-1.0773470373727,1.,1.72957248977424));
#28545=CARTESIAN_POINT('Ctrl Pts',(-1.07234866990252,1.,1.72599406198488));
#28546=CARTESIAN_POINT('Ctrl Pts',(-1.06738966975462,1.,1.72238500928453));
#28547=CARTESIAN_POINT('Ctrl Pts',(-1.06247324680647,1.,1.71874858456904));
#28548=CARTESIAN_POINT('Ctrl Pts',(-1.05760163192479,1.,1.7150865442702));
#28549=CARTESIAN_POINT('Ctrl Pts',(-1.05277517202855,1.,1.71139783543989));
#28550=CARTESIAN_POINT('Ctrl Pts',(-1.04799085404995,1.,1.70767646263649));
#28551=CARTESIAN_POINT('Ctrl Pts',(-1.04324363334554,1.,1.70391338707982));
#28552=CARTESIAN_POINT('Ctrl Pts',(-1.03852922490789,1.,1.70010052930962));
#28553=CARTESIAN_POINT('Ctrl Pts',(-1.03384646003588,1.,1.69623414782771));
#28554=CARTESIAN_POINT('Ctrl Pts',(-1.02919977579147,1.,1.69231840863458));
#28555=CARTESIAN_POINT('Ctrl Pts',(-1.02460180535255,1.,1.68836910178447));
#28556=CARTESIAN_POINT('Ctrl Pts',(-1.02006795074201,1.,1.68440578021706));
#28557=CARTESIAN_POINT('Ctrl Pts',(-1.01561026162773,1.,1.68044289894798));
#28558=CARTESIAN_POINT('Ctrl Pts',(-1.01123236493511,1.,1.67648246776464));
#28559=CARTESIAN_POINT('Ctrl Pts',(-1.00692206696414,1.,1.67250335383293));
#28560=CARTESIAN_POINT('Ctrl Pts',(-1.00265091003727,1.,1.66846059277303));
#28561=CARTESIAN_POINT('Ctrl Pts',(-0.998389654952758,1.,1.66430758030376));
#28562=CARTESIAN_POINT('Ctrl Pts',(-0.994121836661306,1.,1.66001553809947));
#28563=CARTESIAN_POINT('Ctrl Pts',(-0.989855627854165,1.,1.65559044289699));
#28564=CARTESIAN_POINT('Ctrl Pts',(-0.985642622920821,1.,1.65110016612638));
#28565=CARTESIAN_POINT('Ctrl Pts',(-0.981562530939489,1.,1.64665139190656));
#28566=CARTESIAN_POINT('Ctrl Pts',(-0.977689794119416,1.,1.64233990826687));
#28567=CARTESIAN_POINT('Ctrl Pts',(-0.974066058287418,1.,1.63820952658144));
#28568=CARTESIAN_POINT('Ctrl Pts',(-0.970669715997509,1.,1.63420665729798));
#28569=CARTESIAN_POINT('Ctrl Pts',(-0.967387853230345,1.,1.63013849959461));
#28570=CARTESIAN_POINT('Ctrl Pts',(-0.964046107040536,1.,1.62571930670187));
#28571=CARTESIAN_POINT('Ctrl Pts',(-0.960438326101729,1.,1.62061638140221));
#28572=CARTESIAN_POINT('Ctrl Pts',(-0.956354422920671,1.,1.61449324337085));
#28573=CARTESIAN_POINT('Ctrl Pts',(-0.951613284356035,1.,1.60706069896936));
#28574=CARTESIAN_POINT('Ctrl Pts',(-0.946078063315257,1.,1.59810042043673));
#28575=CARTESIAN_POINT('Ctrl Pts',(-0.939646377893399,1.,1.58744937487176));
#28576=CARTESIAN_POINT('Ctrl Pts',(-0.932246680108685,1.,1.57499388382243));
#28577=CARTESIAN_POINT('Ctrl Pts',(-0.923832188944341,1.,1.56065988578893));
#28578=CARTESIAN_POINT('Ctrl Pts',(-0.914375919026456,1.,1.54440491149498));
#28579=CARTESIAN_POINT('Ctrl Pts',(-0.905967409625651,1.,1.52984849887993));
#28580=CARTESIAN_POINT('Ctrl Pts',(-0.899185047483511,1.,1.51805569590094));
#28581=CARTESIAN_POINT('Ctrl Pts',(-0.894452006964543,1.,1.50980486806688));
#28582=CARTESIAN_POINT('Ctrl Pts',(-0.892032620296855,1.,1.5055822144029));
#28583=CARTESIAN_POINT('',(-1.23627494547115,0.,1.81978687191668));
#28584=CARTESIAN_POINT('Origin',(-1.34869019493419,0.,1.73811241238545));
#28585=CARTESIAN_POINT('',(-1.34869019493419,1.,1.73811241238545));
#28586=CARTESIAN_POINT('',(-1.23627494547115,1.,1.81978687191668));
#28587=CARTESIAN_POINT('',(-1.34869019493419,0.,1.73811241238545));
#28588=CARTESIAN_POINT('Ctrl Pts',(-1.15624053661742,-1.,1.31362392696032));
#28589=CARTESIAN_POINT('Ctrl Pts',(-1.15624053661742,1.,1.31362392696032));
#28590=CARTESIAN_POINT('Ctrl Pts',(-1.15950888730809,-1.,1.31722977216397));
#28591=CARTESIAN_POINT('Ctrl Pts',(-1.15950888730809,1.,1.31722977216397));
#28592=CARTESIAN_POINT('Ctrl Pts',(-1.16589330093588,-1.,1.32428080721772));
#28593=CARTESIAN_POINT('Ctrl Pts',(-1.16589330093588,1.,1.32428080721772));
#28594=CARTESIAN_POINT('Ctrl Pts',(-1.17501305789857,-1.,1.33437539347008));
#28595=CARTESIAN_POINT('Ctrl Pts',(-1.17501305789857,1.,1.33437539347008));
#28596=CARTESIAN_POINT('Ctrl Pts',(-1.18625865667441,-1.,1.34687054001093));
#28597=CARTESIAN_POINT('Ctrl Pts',(-1.18625865667441,1.,1.34687054001093));
#28598=CARTESIAN_POINT('Ctrl Pts',(-1.1987959077932,-1.,1.36088705043885));
#28599=CARTESIAN_POINT('Ctrl Pts',(-1.1987959077932,1.,1.36088705043885));
#28600=CARTESIAN_POINT('Ctrl Pts',(-1.20982812925645,-1.,1.37331915607905));
#28601=CARTESIAN_POINT('Ctrl Pts',(-1.20982812925645,1.,1.37331915607905));
#28602=CARTESIAN_POINT('Ctrl Pts',(-1.21938737280852,-1.,1.38420564527715));
#28603=CARTESIAN_POINT('Ctrl Pts',(-1.21938737280852,1.,1.38420564527715));
#28604=CARTESIAN_POINT('Ctrl Pts',(-1.22752961899387,-1.,1.39361389568796));
#28605=CARTESIAN_POINT('Ctrl Pts',(-1.22752961899387,1.,1.39361389568796));
#28606=CARTESIAN_POINT('Ctrl Pts',(-1.23434087290423,-1.,1.40164708206106));
#28607=CARTESIAN_POINT('Ctrl Pts',(-1.23434087290423,1.,1.40164708206106));
#28608=CARTESIAN_POINT('Ctrl Pts',(-1.23994455029534,-1.,1.40845295531283));
#28609=CARTESIAN_POINT('Ctrl Pts',(-1.23994455029534,1.,1.40845295531283));
#28610=CARTESIAN_POINT('Ctrl Pts',(-1.24450600513056,-1.,1.41422913175179));
#28611=CARTESIAN_POINT('Ctrl Pts',(-1.24450600513056,1.,1.41422913175179));
#28612=CARTESIAN_POINT('Ctrl Pts',(-1.24824430986571,-1.,1.41923722596025));
#28613=CARTESIAN_POINT('Ctrl Pts',(-1.24824430986571,1.,1.41923722596025));
#28614=CARTESIAN_POINT('Ctrl Pts',(-1.2514145557001,-1.,1.42378102115575));
#28615=CARTESIAN_POINT('Ctrl Pts',(-1.2514145557001,1.,1.42378102115575));
#28616=CARTESIAN_POINT('Ctrl Pts',(-1.25426945222639,-1.,1.42815938799387));
#28617=CARTESIAN_POINT('Ctrl Pts',(-1.25426945222639,1.,1.42815938799387));
#28618=CARTESIAN_POINT('Ctrl Pts',(-1.25702687965755,-1.,1.43262645609691));
#28619=CARTESIAN_POINT('Ctrl Pts',(-1.25702687965755,1.,1.43262645609691));
#28620=CARTESIAN_POINT('Ctrl Pts',(-1.25983531012005,-1.,1.43734919180848));
#28621=CARTESIAN_POINT('Ctrl Pts',(-1.25983531012005,1.,1.43734919180848));
#28622=CARTESIAN_POINT('Ctrl Pts',(-1.26273903323859,-1.,1.44236470511303));
#28623=CARTESIAN_POINT('Ctrl Pts',(-1.26273903323859,1.,1.44236470511303));
#28624=CARTESIAN_POINT('Ctrl Pts',(-1.26570925118868,-1.,1.44761985001662));
#28625=CARTESIAN_POINT('Ctrl Pts',(-1.26570925118868,1.,1.44761985001662));
#28626=CARTESIAN_POINT('Ctrl Pts',(-1.2686778680489,-1.,1.45301422764247));
#28627=CARTESIAN_POINT('Ctrl Pts',(-1.2686778680489,1.,1.45301422764247));
#28628=CARTESIAN_POINT('Ctrl Pts',(-1.27156805265289,-1.,1.45843906294697));
#28629=CARTESIAN_POINT('Ctrl Pts',(-1.27156805265289,1.,1.45843906294697));
#28630=CARTESIAN_POINT('Ctrl Pts',(-1.27433119897822,-1.,1.46382431332476));
#28631=CARTESIAN_POINT('Ctrl Pts',(-1.27433119897822,1.,1.46382431332476));
#28632=CARTESIAN_POINT('Ctrl Pts',(-1.27696414831089,-1.,1.46916035917133));
#28633=CARTESIAN_POINT('Ctrl Pts',(-1.27696414831089,1.,1.46916035917133));
#28634=CARTESIAN_POINT('Ctrl Pts',(-1.2794891824849,-1.,1.4744717526707));
#28635=CARTESIAN_POINT('Ctrl Pts',(-1.2794891824849,1.,1.4744717526707));
#28636=CARTESIAN_POINT('Ctrl Pts',(-1.28194158939517,-1.,1.47980070347095));
#28637=CARTESIAN_POINT('Ctrl Pts',(-1.28194158939517,1.,1.47980070347095));
#28638=CARTESIAN_POINT('Ctrl Pts',(-1.28435533880201,-1.,1.4851881711891));
#28639=CARTESIAN_POINT('Ctrl Pts',(-1.28435533880201,1.,1.4851881711891));
#28640=CARTESIAN_POINT('Ctrl Pts',(-1.2867467611644,-1.,1.4906522831278));
#28641=CARTESIAN_POINT('Ctrl Pts',(-1.2867467611644,1.,1.4906522831278));
#28642=CARTESIAN_POINT('Ctrl Pts',(-1.28911506584254,-1.,1.49618896881754));
#28643=CARTESIAN_POINT('Ctrl Pts',(-1.28911506584254,1.,1.49618896881754));
#28644=CARTESIAN_POINT('Ctrl Pts',(-1.29145022885181,-1.,1.50178230149776));
#28645=CARTESIAN_POINT('Ctrl Pts',(-1.29145022885181,1.,1.50178230149776));
#28646=CARTESIAN_POINT('Ctrl Pts',(-1.29373841372842,-1.,1.50741159078365));
#28647=CARTESIAN_POINT('Ctrl Pts',(-1.29373841372842,1.,1.50741159078365));
#28648=CARTESIAN_POINT('Ctrl Pts',(-1.29596850710509,-1.,1.51305994241402));
#28649=CARTESIAN_POINT('Ctrl Pts',(-1.29596850710509,1.,1.51305994241402));
#28650=CARTESIAN_POINT('Ctrl Pts',(-1.29813791800747,-1.,1.51872184912724));
#28651=CARTESIAN_POINT('Ctrl Pts',(-1.29813791800747,1.,1.51872184912724));
#28652=CARTESIAN_POINT('Ctrl Pts',(-1.30024984366328,-1.,1.52439957861062));
#28653=CARTESIAN_POINT('Ctrl Pts',(-1.30024984366328,1.,1.52439957861062));
#28654=CARTESIAN_POINT('Ctrl Pts',(-1.30231064395568,-1.,1.53009970283891));
#28655=CARTESIAN_POINT('Ctrl Pts',(-1.30231064395568,1.,1.53009970283891));
#28656=CARTESIAN_POINT('Ctrl Pts',(-1.30432735639489,-1.,1.53582981268977));
#28657=CARTESIAN_POINT('Ctrl Pts',(-1.30432735639489,1.,1.53582981268977));
#28658=CARTESIAN_POINT('Ctrl Pts',(-1.30630475189556,-1.,1.54159462645432));
#28659=CARTESIAN_POINT('Ctrl Pts',(-1.30630475189556,1.,1.54159462645432));
#28660=CARTESIAN_POINT('Ctrl Pts',(-1.30824393907473,-1.,1.54739413957185));
#28661=CARTESIAN_POINT('Ctrl Pts',(-1.30824393907473,1.,1.54739413957185));
#28662=CARTESIAN_POINT('Ctrl Pts',(-1.31014393684222,-1.,1.55322568759481));
#28663=CARTESIAN_POINT('Ctrl Pts',(-1.31014393684222,1.,1.55322568759481));
#28664=CARTESIAN_POINT('Ctrl Pts',(-1.31200264341696,-1.,1.55908521254821));
#28665=CARTESIAN_POINT('Ctrl Pts',(-1.31200264341696,1.,1.55908521254821));
#28666=CARTESIAN_POINT('Ctrl Pts',(-1.31381795281002,-1.,1.56496872402353));
#28667=CARTESIAN_POINT('Ctrl Pts',(-1.31381795281002,1.,1.56496872402353));
#28668=CARTESIAN_POINT('Ctrl Pts',(-1.31558903860016,-1.,1.57087397835723));
#28669=CARTESIAN_POINT('Ctrl Pts',(-1.31558903860016,1.,1.57087397835723));
#28670=CARTESIAN_POINT('Ctrl Pts',(-1.31731642317187,-1.,1.5768005650559));
#28671=CARTESIAN_POINT('Ctrl Pts',(-1.31731642317187,1.,1.5768005650559));
#28672=CARTESIAN_POINT('Ctrl Pts',(-1.31900135021432,-1.,1.58274907898834));
#28673=CARTESIAN_POINT('Ctrl Pts',(-1.31900135021432,1.,1.58274907898834));
#28674=CARTESIAN_POINT('Ctrl Pts',(-1.32064537110892,-1.,1.58872057258245));
#28675=CARTESIAN_POINT('Ctrl Pts',(-1.32064537110892,1.,1.58872057258245));
#28676=CARTESIAN_POINT('Ctrl Pts',(-1.32224985747682,-1.,1.59471591079403));
#28677=CARTESIAN_POINT('Ctrl Pts',(-1.32224985747682,1.,1.59471591079403));
#28678=CARTESIAN_POINT('Ctrl Pts',(-1.32381550858256,-1.,1.60073511858687));
#28679=CARTESIAN_POINT('Ctrl Pts',(-1.32381550858256,1.,1.60073511858687));
#28680=CARTESIAN_POINT('Ctrl Pts',(-1.32534250785782,-1.,1.60677758290954));
#28681=CARTESIAN_POINT('Ctrl Pts',(-1.32534250785782,1.,1.60677758290954));
#28682=CARTESIAN_POINT('Ctrl Pts',(-1.32683074483356,-1.,1.6128423401575));
#28683=CARTESIAN_POINT('Ctrl Pts',(-1.32683074483356,1.,1.6128423401575));
#28684=CARTESIAN_POINT('Ctrl Pts',(-1.32828000610449,-1.,1.61892832270724));
#28685=CARTESIAN_POINT('Ctrl Pts',(-1.32828000610449,1.,1.61892832270724));
#28686=CARTESIAN_POINT('Ctrl Pts',(-1.3296901950568,-1.,1.62503464209797));
#28687=CARTESIAN_POINT('Ctrl Pts',(-1.3296901950568,1.,1.62503464209797));
#28688=CARTESIAN_POINT('Ctrl Pts',(-1.33106149345645,-1.,1.63116079730923));
#28689=CARTESIAN_POINT('Ctrl Pts',(-1.33106149345645,1.,1.63116079730923));
#28690=CARTESIAN_POINT('Ctrl Pts',(-1.33239425103724,-1.,1.63730653475089));
#28691=CARTESIAN_POINT('Ctrl Pts',(-1.33239425103724,1.,1.63730653475089));
#28692=CARTESIAN_POINT('Ctrl Pts',(-1.33368890676572,-1.,1.6434717485603));
#28693=CARTESIAN_POINT('Ctrl Pts',(-1.33368890676572,1.,1.6434717485603));
#28694=CARTESIAN_POINT('Ctrl Pts',(-1.33494590467993,-1.,1.6496563728683));
#28695=CARTESIAN_POINT('Ctrl Pts',(-1.33494590467993,1.,1.6496563728683));
#28696=CARTESIAN_POINT('Ctrl Pts',(-1.33616559745172,-1.,1.65586025952593));
#28697=CARTESIAN_POINT('Ctrl Pts',(-1.33616559745172,1.,1.65586025952593));
#28698=CARTESIAN_POINT('Ctrl Pts',(-1.33734820885262,-1.,1.66208312541983));
#28699=CARTESIAN_POINT('Ctrl Pts',(-1.33734820885262,1.,1.66208312541983));
#28700=CARTESIAN_POINT('Ctrl Pts',(-1.33849388654388,-1.,1.66832460783989));
#28701=CARTESIAN_POINT('Ctrl Pts',(-1.33849388654388,1.,1.66832460783989));
#28702=CARTESIAN_POINT('Ctrl Pts',(-1.3396027347034,-1.,1.67458429426086));
#28703=CARTESIAN_POINT('Ctrl Pts',(-1.3396027347034,1.,1.67458429426086));
#28704=CARTESIAN_POINT('Ctrl Pts',(-1.34067485185203,-1.,1.68086176030362));
#28705=CARTESIAN_POINT('Ctrl Pts',(-1.34067485185203,1.,1.68086176030362));
#28706=CARTESIAN_POINT('Ctrl Pts',(-1.341710374848,-1.,1.68715660868764));
#28707=CARTESIAN_POINT('Ctrl Pts',(-1.341710374848,1.,1.68715660868764));
#28708=CARTESIAN_POINT('Ctrl Pts',(-1.34270948206319,-1.,1.6934684849687));
#28709=CARTESIAN_POINT('Ctrl Pts',(-1.34270948206319,1.,1.6934684849687));
#28710=CARTESIAN_POINT('Ctrl Pts',(-1.34367237124483,-1.,1.69979707754427));
#28711=CARTESIAN_POINT('Ctrl Pts',(-1.34367237124483,1.,1.69979707754427));
#28712=CARTESIAN_POINT('Ctrl Pts',(-1.34459924533831,-1.,1.70614212266738));
#28713=CARTESIAN_POINT('Ctrl Pts',(-1.34459924533831,1.,1.70614212266738));
#28714=CARTESIAN_POINT('Ctrl Pts',(-1.34549029589416,-1.,1.71250340686822));
#28715=CARTESIAN_POINT('Ctrl Pts',(-1.34549029589416,1.,1.71250340686822));
#28716=CARTESIAN_POINT('Ctrl Pts',(-1.34634568653227,-1.,1.7188807715049));
#28717=CARTESIAN_POINT('Ctrl Pts',(-1.34634568653227,1.,1.7188807715049));
#28718=CARTESIAN_POINT('Ctrl Pts',(-1.34716554819527,-1.,1.72527410680674));
#28719=CARTESIAN_POINT('Ctrl Pts',(-1.34716554819527,1.,1.72527410680674));
#28720=CARTESIAN_POINT('Ctrl Pts',(-1.34779309152035,-1.,1.7304014965394));
#28721=CARTESIAN_POINT('Ctrl Pts',(-1.34779309152035,1.,1.7304014965394));
#28722=CARTESIAN_POINT('Ctrl Pts',(-1.34824783112887,-1.,1.73425417885907));
#28723=CARTESIAN_POINT('Ctrl Pts',(-1.34824783112887,1.,1.73425417885907));
#28724=CARTESIAN_POINT('Ctrl Pts',(-1.34854391898045,-1.,1.73682580585691));
#28725=CARTESIAN_POINT('Ctrl Pts',(-1.34854391898045,1.,1.73682580585691));
#28726=CARTESIAN_POINT('Ctrl Pts',(-1.34869019493419,-1.,1.73811241238545));
#28727=CARTESIAN_POINT('Ctrl Pts',(-1.34869019493419,1.,1.73811241238545));
#28728=CARTESIAN_POINT('',(-1.15624053661742,1.,1.31362392696032));
#28729=CARTESIAN_POINT('Ctrl Pts',(-1.15624053661742,1.,1.31362392696032));
#28730=CARTESIAN_POINT('Ctrl Pts',(-1.15950888730809,1.,1.31722977216397));
#28731=CARTESIAN_POINT('Ctrl Pts',(-1.16589330093588,1.,1.32428080721772));
#28732=CARTESIAN_POINT('Ctrl Pts',(-1.17501305789857,1.,1.33437539347008));
#28733=CARTESIAN_POINT('Ctrl Pts',(-1.18625865667441,1.,1.34687054001093));
#28734=CARTESIAN_POINT('Ctrl Pts',(-1.1987959077932,1.,1.36088705043885));
#28735=CARTESIAN_POINT('Ctrl Pts',(-1.20982812925645,1.,1.37331915607905));
#28736=CARTESIAN_POINT('Ctrl Pts',(-1.21938737280852,1.,1.38420564527715));
#28737=CARTESIAN_POINT('Ctrl Pts',(-1.22752961899387,1.,1.39361389568796));
#28738=CARTESIAN_POINT('Ctrl Pts',(-1.23434087290423,1.,1.40164708206106));
#28739=CARTESIAN_POINT('Ctrl Pts',(-1.23994455029534,1.,1.40845295531283));
#28740=CARTESIAN_POINT('Ctrl Pts',(-1.24450600513056,1.,1.41422913175179));
#28741=CARTESIAN_POINT('Ctrl Pts',(-1.24824430986571,1.,1.41923722596025));
#28742=CARTESIAN_POINT('Ctrl Pts',(-1.2514145557001,1.,1.42378102115575));
#28743=CARTESIAN_POINT('Ctrl Pts',(-1.25426945222639,1.,1.42815938799387));
#28744=CARTESIAN_POINT('Ctrl Pts',(-1.25702687965755,1.,1.43262645609691));
#28745=CARTESIAN_POINT('Ctrl Pts',(-1.25983531012005,1.,1.43734919180848));
#28746=CARTESIAN_POINT('Ctrl Pts',(-1.26273903323859,1.,1.44236470511303));
#28747=CARTESIAN_POINT('Ctrl Pts',(-1.26570925118868,1.,1.44761985001662));
#28748=CARTESIAN_POINT('Ctrl Pts',(-1.2686778680489,1.,1.45301422764247));
#28749=CARTESIAN_POINT('Ctrl Pts',(-1.27156805265289,1.,1.45843906294697));
#28750=CARTESIAN_POINT('Ctrl Pts',(-1.27433119897822,1.,1.46382431332476));
#28751=CARTESIAN_POINT('Ctrl Pts',(-1.27696414831089,1.,1.46916035917133));
#28752=CARTESIAN_POINT('Ctrl Pts',(-1.2794891824849,1.,1.4744717526707));
#28753=CARTESIAN_POINT('Ctrl Pts',(-1.28194158939517,1.,1.47980070347095));
#28754=CARTESIAN_POINT('Ctrl Pts',(-1.28435533880201,1.,1.4851881711891));
#28755=CARTESIAN_POINT('Ctrl Pts',(-1.2867467611644,1.,1.4906522831278));
#28756=CARTESIAN_POINT('Ctrl Pts',(-1.28911506584254,1.,1.49618896881754));
#28757=CARTESIAN_POINT('Ctrl Pts',(-1.29145022885181,1.,1.50178230149776));
#28758=CARTESIAN_POINT('Ctrl Pts',(-1.29373841372842,1.,1.50741159078365));
#28759=CARTESIAN_POINT('Ctrl Pts',(-1.29596850710509,1.,1.51305994241402));
#28760=CARTESIAN_POINT('Ctrl Pts',(-1.29813791800747,1.,1.51872184912724));
#28761=CARTESIAN_POINT('Ctrl Pts',(-1.30024984366328,1.,1.52439957861062));
#28762=CARTESIAN_POINT('Ctrl Pts',(-1.30231064395568,1.,1.53009970283891));
#28763=CARTESIAN_POINT('Ctrl Pts',(-1.30432735639489,1.,1.53582981268977));
#28764=CARTESIAN_POINT('Ctrl Pts',(-1.30630475189556,1.,1.54159462645432));
#28765=CARTESIAN_POINT('Ctrl Pts',(-1.30824393907473,1.,1.54739413957185));
#28766=CARTESIAN_POINT('Ctrl Pts',(-1.31014393684222,1.,1.55322568759481));
#28767=CARTESIAN_POINT('Ctrl Pts',(-1.31200264341696,1.,1.55908521254821));
#28768=CARTESIAN_POINT('Ctrl Pts',(-1.31381795281002,1.,1.56496872402353));
#28769=CARTESIAN_POINT('Ctrl Pts',(-1.31558903860016,1.,1.57087397835723));
#28770=CARTESIAN_POINT('Ctrl Pts',(-1.31731642317187,1.,1.5768005650559));
#28771=CARTESIAN_POINT('Ctrl Pts',(-1.31900135021432,1.,1.58274907898834));
#28772=CARTESIAN_POINT('Ctrl Pts',(-1.32064537110892,1.,1.58872057258245));
#28773=CARTESIAN_POINT('Ctrl Pts',(-1.32224985747682,1.,1.59471591079403));
#28774=CARTESIAN_POINT('Ctrl Pts',(-1.32381550858256,1.,1.60073511858687));
#28775=CARTESIAN_POINT('Ctrl Pts',(-1.32534250785782,1.,1.60677758290954));
#28776=CARTESIAN_POINT('Ctrl Pts',(-1.32683074483356,1.,1.6128423401575));
#28777=CARTESIAN_POINT('Ctrl Pts',(-1.32828000610449,1.,1.61892832270724));
#28778=CARTESIAN_POINT('Ctrl Pts',(-1.3296901950568,1.,1.62503464209797));
#28779=CARTESIAN_POINT('Ctrl Pts',(-1.33106149345645,1.,1.63116079730923));
#28780=CARTESIAN_POINT('Ctrl Pts',(-1.33239425103724,1.,1.63730653475089));
#28781=CARTESIAN_POINT('Ctrl Pts',(-1.33368890676572,1.,1.6434717485603));
#28782=CARTESIAN_POINT('Ctrl Pts',(-1.33494590467993,1.,1.6496563728683));
#28783=CARTESIAN_POINT('Ctrl Pts',(-1.33616559745172,1.,1.65586025952593));
#28784=CARTESIAN_POINT('Ctrl Pts',(-1.33734820885262,1.,1.66208312541983));
#28785=CARTESIAN_POINT('Ctrl Pts',(-1.33849388654388,1.,1.66832460783989));
#28786=CARTESIAN_POINT('Ctrl Pts',(-1.3396027347034,1.,1.67458429426086));
#28787=CARTESIAN_POINT('Ctrl Pts',(-1.34067485185203,1.,1.68086176030362));
#28788=CARTESIAN_POINT('Ctrl Pts',(-1.341710374848,1.,1.68715660868764));
#28789=CARTESIAN_POINT('Ctrl Pts',(-1.34270948206319,1.,1.6934684849687));
#28790=CARTESIAN_POINT('Ctrl Pts',(-1.34367237124483,1.,1.69979707754427));
#28791=CARTESIAN_POINT('Ctrl Pts',(-1.34459924533831,1.,1.70614212266738));
#28792=CARTESIAN_POINT('Ctrl Pts',(-1.34549029589416,1.,1.71250340686822));
#28793=CARTESIAN_POINT('Ctrl Pts',(-1.34634568653227,1.,1.7188807715049));
#28794=CARTESIAN_POINT('Ctrl Pts',(-1.34716554819527,1.,1.72527410680674));
#28795=CARTESIAN_POINT('Ctrl Pts',(-1.34779309152035,1.,1.7304014965394));
#28796=CARTESIAN_POINT('Ctrl Pts',(-1.34824783112887,1.,1.73425417885907));
#28797=CARTESIAN_POINT('Ctrl Pts',(-1.34854391898045,1.,1.73682580585691));
#28798=CARTESIAN_POINT('Ctrl Pts',(-1.34869019493419,1.,1.73811241238545));
#28799=CARTESIAN_POINT('',(-1.15624053661742,0.,1.31362392696032));
#28800=CARTESIAN_POINT('Origin',(0.,0.,0.));
#28801=CARTESIAN_POINT('',(-1.31362392696033,1.,1.15624053661742));
#28802=CARTESIAN_POINT('Origin',(0.,1.,0.));
#28803=CARTESIAN_POINT('',(-1.31362392696033,0.,1.15624053661742));
#28804=CARTESIAN_POINT('Ctrl Pts',(-1.73811241238545,-1.,1.34869019493419));
#28805=CARTESIAN_POINT('Ctrl Pts',(-1.73811241238545,1.,1.34869019493419));
#28806=CARTESIAN_POINT('Ctrl Pts',(-1.73682580585819,-1.,1.34854391898145));
#28807=CARTESIAN_POINT('Ctrl Pts',(-1.73682580585819,1.,1.34854391898145));
#28808=CARTESIAN_POINT('Ctrl Pts',(-1.73425417886255,-1.,1.34824783113158));
#28809=CARTESIAN_POINT('Ctrl Pts',(-1.73425417886255,1.,1.34824783113158));
#28810=CARTESIAN_POINT('Ctrl Pts',(-1.73040149654497,-1.,1.3477930915247));
#28811=CARTESIAN_POINT('Ctrl Pts',(-1.73040149654497,1.,1.3477930915247));
#28812=CARTESIAN_POINT('Ctrl Pts',(-1.72527410681298,-1.,1.34716554820013));
#28813=CARTESIAN_POINT('Ctrl Pts',(-1.72527410681298,1.,1.34716554820013));
#28814=CARTESIAN_POINT('Ctrl Pts',(-1.7188807715095,-1.,1.34634568653586));
#28815=CARTESIAN_POINT('Ctrl Pts',(-1.7188807715095,1.,1.34634568653586));
#28816=CARTESIAN_POINT('Ctrl Pts',(-1.71250340687011,-1.,1.34549029589563));
#28817=CARTESIAN_POINT('Ctrl Pts',(-1.71250340687011,1.,1.34549029589563));
#28818=CARTESIAN_POINT('Ctrl Pts',(-1.70614212266676,-1.,1.34459924533783));
#28819=CARTESIAN_POINT('Ctrl Pts',(-1.70614212266676,1.,1.34459924533783));
#28820=CARTESIAN_POINT('Ctrl Pts',(-1.69979707754221,-1.,1.34367237124322));
#28821=CARTESIAN_POINT('Ctrl Pts',(-1.69979707754221,1.,1.34367237124322));
#28822=CARTESIAN_POINT('Ctrl Pts',(-1.6934684849664,-1.,1.34270948206139));
#28823=CARTESIAN_POINT('Ctrl Pts',(-1.6934684849664,1.,1.34270948206139));
#28824=CARTESIAN_POINT('Ctrl Pts',(-1.68715660868602,-1.,1.34171037484673));
#28825=CARTESIAN_POINT('Ctrl Pts',(-1.68715660868602,1.,1.34171037484673));
#28826=CARTESIAN_POINT('Ctrl Pts',(-1.68086176030308,-1.,1.3406748518516));
#28827=CARTESIAN_POINT('Ctrl Pts',(-1.68086176030308,1.,1.3406748518516));
#28828=CARTESIAN_POINT('Ctrl Pts',(-1.67458429426126,-1.,1.33960273470372));
#28829=CARTESIAN_POINT('Ctrl Pts',(-1.67458429426126,1.,1.33960273470372));
#28830=CARTESIAN_POINT('Ctrl Pts',(-1.66832460784078,-1.,1.33849388654458));
#28831=CARTESIAN_POINT('Ctrl Pts',(-1.66832460784078,1.,1.33849388654458));
#28832=CARTESIAN_POINT('Ctrl Pts',(-1.66208312542073,-1.,1.33734820885331));
#28833=CARTESIAN_POINT('Ctrl Pts',(-1.66208312542073,1.,1.33734820885331));
#28834=CARTESIAN_POINT('Ctrl Pts',(-1.65586025952651,-1.,1.33616559745217));
#28835=CARTESIAN_POINT('Ctrl Pts',(-1.65586025952651,1.,1.33616559745217));
#28836=CARTESIAN_POINT('Ctrl Pts',(-1.64965637286843,-1.,1.33494590468003));
#28837=CARTESIAN_POINT('Ctrl Pts',(-1.64965637286843,1.,1.33494590468003));
#28838=CARTESIAN_POINT('Ctrl Pts',(-1.64347174856007,-1.,1.33368890676554));
#28839=CARTESIAN_POINT('Ctrl Pts',(-1.64347174856007,1.,1.33368890676554));
#28840=CARTESIAN_POINT('Ctrl Pts',(-1.6373065347505,-1.,1.33239425103694));
#28841=CARTESIAN_POINT('Ctrl Pts',(-1.6373065347505,1.,1.33239425103694));
#28842=CARTESIAN_POINT('Ctrl Pts',(-1.63116079730887,-1.,1.33106149345618));
#28843=CARTESIAN_POINT('Ctrl Pts',(-1.63116079730887,1.,1.33106149345618));
#28844=CARTESIAN_POINT('Ctrl Pts',(-1.62503464209777,-1.,1.32969019505665));
#28845=CARTESIAN_POINT('Ctrl Pts',(-1.62503464209777,1.,1.32969019505665));
#28846=CARTESIAN_POINT('Ctrl Pts',(-1.61892832270723,-1.,1.32828000610448));
#28847=CARTESIAN_POINT('Ctrl Pts',(-1.61892832270723,1.,1.32828000610448));
#28848=CARTESIAN_POINT('Ctrl Pts',(-1.61284234015762,-1.,1.32683074483365));
#28849=CARTESIAN_POINT('Ctrl Pts',(-1.61284234015762,1.,1.32683074483365));
#28850=CARTESIAN_POINT('Ctrl Pts',(-1.6067775829097,-1.,1.32534250785794));
#28851=CARTESIAN_POINT('Ctrl Pts',(-1.6067775829097,1.,1.32534250785794));
#28852=CARTESIAN_POINT('Ctrl Pts',(-1.600735118587,-1.,1.32381550858266));
#28853=CARTESIAN_POINT('Ctrl Pts',(-1.600735118587,1.,1.32381550858266));
#28854=CARTESIAN_POINT('Ctrl Pts',(-1.59471591079408,-1.,1.32224985747686));
#28855=CARTESIAN_POINT('Ctrl Pts',(-1.59471591079408,1.,1.32224985747686));
#28856=CARTESIAN_POINT('Ctrl Pts',(-1.58872057258244,-1.,1.32064537110891));
#28857=CARTESIAN_POINT('Ctrl Pts',(-1.58872057258244,1.,1.32064537110891));
#28858=CARTESIAN_POINT('Ctrl Pts',(-1.58274907898829,-1.,1.31900135021428));
#28859=CARTESIAN_POINT('Ctrl Pts',(-1.58274907898829,1.,1.31900135021428));
#28860=CARTESIAN_POINT('Ctrl Pts',(-1.57680056505585,-1.,1.31731642317183));
#28861=CARTESIAN_POINT('Ctrl Pts',(-1.57680056505585,1.,1.31731642317183));
#28862=CARTESIAN_POINT('Ctrl Pts',(-1.57087397835721,-1.,1.31558903860015));
#28863=CARTESIAN_POINT('Ctrl Pts',(-1.57087397835721,1.,1.31558903860015));
#28864=CARTESIAN_POINT('Ctrl Pts',(-1.56496872402352,-1.,1.31381795281002));
#28865=CARTESIAN_POINT('Ctrl Pts',(-1.56496872402352,1.,1.31381795281002));
#28866=CARTESIAN_POINT('Ctrl Pts',(-1.55908521254822,-1.,1.31200264341696));
#28867=CARTESIAN_POINT('Ctrl Pts',(-1.55908521254822,1.,1.31200264341696));
#28868=CARTESIAN_POINT('Ctrl Pts',(-1.55322568759481,-1.,1.31014393684221));
#28869=CARTESIAN_POINT('Ctrl Pts',(-1.55322568759481,1.,1.31014393684221));
#28870=CARTESIAN_POINT('Ctrl Pts',(-1.54739413957183,-1.,1.30824393907471));
#28871=CARTESIAN_POINT('Ctrl Pts',(-1.54739413957183,1.,1.30824393907471));
#28872=CARTESIAN_POINT('Ctrl Pts',(-1.54159462645428,-1.,1.30630475189553));
#28873=CARTESIAN_POINT('Ctrl Pts',(-1.54159462645428,1.,1.30630475189553));
#28874=CARTESIAN_POINT('Ctrl Pts',(-1.53582981268976,-1.,1.30432735639487));
#28875=CARTESIAN_POINT('Ctrl Pts',(-1.53582981268976,1.,1.30432735639487));
#28876=CARTESIAN_POINT('Ctrl Pts',(-1.53009970283893,-1.,1.3023106439557));
#28877=CARTESIAN_POINT('Ctrl Pts',(-1.53009970283893,1.,1.3023106439557));
#28878=CARTESIAN_POINT('Ctrl Pts',(-1.5243995786107,-1.,1.30024984366334));
#28879=CARTESIAN_POINT('Ctrl Pts',(-1.5243995786107,1.,1.30024984366334));
#28880=CARTESIAN_POINT('Ctrl Pts',(-1.51872184912735,-1.,1.29813791800757));
#28881=CARTESIAN_POINT('Ctrl Pts',(-1.51872184912735,1.,1.29813791800757));
#28882=CARTESIAN_POINT('Ctrl Pts',(-1.51305994241412,-1.,1.29596850710518));
#28883=CARTESIAN_POINT('Ctrl Pts',(-1.51305994241412,1.,1.29596850710518));
#28884=CARTESIAN_POINT('Ctrl Pts',(-1.50741159078367,-1.,1.29373841372843));
#28885=CARTESIAN_POINT('Ctrl Pts',(-1.50741159078367,1.,1.29373841372843));
#28886=CARTESIAN_POINT('Ctrl Pts',(-1.50178230149764,-1.,1.29145022885171));
#28887=CARTESIAN_POINT('Ctrl Pts',(-1.50178230149764,1.,1.29145022885171));
#28888=CARTESIAN_POINT('Ctrl Pts',(-1.49618896881729,-1.,1.28911506584232));
#28889=CARTESIAN_POINT('Ctrl Pts',(-1.49618896881729,1.,1.28911506584232));
#28890=CARTESIAN_POINT('Ctrl Pts',(-1.4906522831275,-1.,1.28674676116415));
#28891=CARTESIAN_POINT('Ctrl Pts',(-1.4906522831275,1.,1.28674676116415));
#28892=CARTESIAN_POINT('Ctrl Pts',(-1.48518817118891,-1.,1.28435533880184));
#28893=CARTESIAN_POINT('Ctrl Pts',(-1.48518817118891,1.,1.28435533880184));
#28894=CARTESIAN_POINT('Ctrl Pts',(-1.47980070347102,-1.,1.28194158939522));
#28895=CARTESIAN_POINT('Ctrl Pts',(-1.47980070347102,1.,1.28194158939522));
#28896=CARTESIAN_POINT('Ctrl Pts',(-1.4744717526711,-1.,1.27948918248524));
#28897=CARTESIAN_POINT('Ctrl Pts',(-1.4744717526711,1.,1.27948918248524));
#28898=CARTESIAN_POINT('Ctrl Pts',(-1.46916035917197,-1.,1.27696414831144));
#28899=CARTESIAN_POINT('Ctrl Pts',(-1.46916035917197,1.,1.27696414831144));
#28900=CARTESIAN_POINT('Ctrl Pts',(-1.4638243133254,-1.,1.27433119897877));
#28901=CARTESIAN_POINT('Ctrl Pts',(-1.4638243133254,1.,1.27433119897877));
#28902=CARTESIAN_POINT('Ctrl Pts',(-1.45843906294725,-1.,1.27156805265312));
#28903=CARTESIAN_POINT('Ctrl Pts',(-1.45843906294725,1.,1.27156805265312));
#28904=CARTESIAN_POINT('Ctrl Pts',(-1.45301422764205,-1.,1.26867786804854));
#28905=CARTESIAN_POINT('Ctrl Pts',(-1.45301422764205,1.,1.26867786804854));
#28906=CARTESIAN_POINT('Ctrl Pts',(-1.44761985001544,-1.,1.26570925118767));
#28907=CARTESIAN_POINT('Ctrl Pts',(-1.44761985001544,1.,1.26570925118767));
#28908=CARTESIAN_POINT('Ctrl Pts',(-1.44236470511145,-1.,1.26273903323723));
#28909=CARTESIAN_POINT('Ctrl Pts',(-1.44236470511145,1.,1.26273903323723));
#28910=CARTESIAN_POINT('Ctrl Pts',(-1.43734919180719,-1.,1.25983531011894));
#28911=CARTESIAN_POINT('Ctrl Pts',(-1.43734919180719,1.,1.25983531011894));
#28912=CARTESIAN_POINT('Ctrl Pts',(-1.43262645609679,-1.,1.25702687965744));
#28913=CARTESIAN_POINT('Ctrl Pts',(-1.43262645609679,1.,1.25702687965744));
#28914=CARTESIAN_POINT('Ctrl Pts',(-1.42815938799555,-1.,1.25426945222783));
#28915=CARTESIAN_POINT('Ctrl Pts',(-1.42815938799555,1.,1.25426945222783));
#28916=CARTESIAN_POINT('Ctrl Pts',(-1.42378102115911,-1.,1.25141455570299));
#28917=CARTESIAN_POINT('Ctrl Pts',(-1.42378102115911,1.,1.25141455570299));
#28918=CARTESIAN_POINT('Ctrl Pts',(-1.41923722596421,-1.,1.24824430986911));
#28919=CARTESIAN_POINT('Ctrl Pts',(-1.41923722596421,1.,1.24824430986911));
#28920=CARTESIAN_POINT('Ctrl Pts',(-1.41422913175437,-1.,1.24450600513278));
#28921=CARTESIAN_POINT('Ctrl Pts',(-1.41422913175437,1.,1.24450600513278));
#28922=CARTESIAN_POINT('Ctrl Pts',(-1.40845295531151,-1.,1.23994455029421));
#28923=CARTESIAN_POINT('Ctrl Pts',(-1.40845295531151,1.,1.23994455029421));
#28924=CARTESIAN_POINT('Ctrl Pts',(-1.40164708205345,-1.,1.23434087289768));
#28925=CARTESIAN_POINT('Ctrl Pts',(-1.40164708205345,1.,1.23434087289768));
#28926=CARTESIAN_POINT('Ctrl Pts',(-1.39361389567257,-1.,1.22752961898063));
#28927=CARTESIAN_POINT('Ctrl Pts',(-1.39361389567257,1.,1.22752961898063));
#28928=CARTESIAN_POINT('Ctrl Pts',(-1.38420564525391,-1.,1.21938737278853));
#28929=CARTESIAN_POINT('Ctrl Pts',(-1.38420564525391,1.,1.21938737278853));
#28930=CARTESIAN_POINT('Ctrl Pts',(-1.37331915604962,-1.,1.20982812923113));
#28931=CARTESIAN_POINT('Ctrl Pts',(-1.37331915604962,1.,1.20982812923113));
#28932=CARTESIAN_POINT('Ctrl Pts',(-1.36088705040677,-1.,1.1987959077656));
#28933=CARTESIAN_POINT('Ctrl Pts',(-1.36088705040677,1.,1.1987959077656));
#28934=CARTESIAN_POINT('Ctrl Pts',(-1.34687053998157,-1.,1.18625865664915));
#28935=CARTESIAN_POINT('Ctrl Pts',(-1.34687053998157,1.,1.18625865664915));
#28936=CARTESIAN_POINT('Ctrl Pts',(-1.33437539344842,-1.,1.17501305787994));
#28937=CARTESIAN_POINT('Ctrl Pts',(-1.33437539344842,1.,1.17501305787994));
#28938=CARTESIAN_POINT('Ctrl Pts',(-1.32428080720544,-1.,1.16589330092532));
#28939=CARTESIAN_POINT('Ctrl Pts',(-1.32428080720544,1.,1.16589330092532));
#28940=CARTESIAN_POINT('Ctrl Pts',(-1.3172297721596,-1.,1.15950888730433));
#28941=CARTESIAN_POINT('Ctrl Pts',(-1.3172297721596,1.,1.15950888730433));
#28942=CARTESIAN_POINT('Ctrl Pts',(-1.31362392696033,-1.,1.15624053661742));
#28943=CARTESIAN_POINT('Ctrl Pts',(-1.31362392696033,1.,1.15624053661742));
#28944=CARTESIAN_POINT('',(-1.73811241238545,1.,1.34869019493419));
#28945=CARTESIAN_POINT('Ctrl Pts',(-1.73811241238545,1.,1.34869019493419));
#28946=CARTESIAN_POINT('Ctrl Pts',(-1.73682580585819,1.,1.34854391898145));
#28947=CARTESIAN_POINT('Ctrl Pts',(-1.73425417886255,1.,1.34824783113158));
#28948=CARTESIAN_POINT('Ctrl Pts',(-1.73040149654497,1.,1.3477930915247));
#28949=CARTESIAN_POINT('Ctrl Pts',(-1.72527410681298,1.,1.34716554820013));
#28950=CARTESIAN_POINT('Ctrl Pts',(-1.7188807715095,1.,1.34634568653586));
#28951=CARTESIAN_POINT('Ctrl Pts',(-1.71250340687011,1.,1.34549029589563));
#28952=CARTESIAN_POINT('Ctrl Pts',(-1.70614212266676,1.,1.34459924533783));
#28953=CARTESIAN_POINT('Ctrl Pts',(-1.69979707754221,1.,1.34367237124322));
#28954=CARTESIAN_POINT('Ctrl Pts',(-1.6934684849664,1.,1.34270948206139));
#28955=CARTESIAN_POINT('Ctrl Pts',(-1.68715660868602,1.,1.34171037484673));
#28956=CARTESIAN_POINT('Ctrl Pts',(-1.68086176030308,1.,1.3406748518516));
#28957=CARTESIAN_POINT('Ctrl Pts',(-1.67458429426126,1.,1.33960273470372));
#28958=CARTESIAN_POINT('Ctrl Pts',(-1.66832460784078,1.,1.33849388654458));
#28959=CARTESIAN_POINT('Ctrl Pts',(-1.66208312542073,1.,1.33734820885331));
#28960=CARTESIAN_POINT('Ctrl Pts',(-1.65586025952651,1.,1.33616559745217));
#28961=CARTESIAN_POINT('Ctrl Pts',(-1.64965637286843,1.,1.33494590468003));
#28962=CARTESIAN_POINT('Ctrl Pts',(-1.64347174856007,1.,1.33368890676554));
#28963=CARTESIAN_POINT('Ctrl Pts',(-1.6373065347505,1.,1.33239425103694));
#28964=CARTESIAN_POINT('Ctrl Pts',(-1.63116079730887,1.,1.33106149345618));
#28965=CARTESIAN_POINT('Ctrl Pts',(-1.62503464209777,1.,1.32969019505665));
#28966=CARTESIAN_POINT('Ctrl Pts',(-1.61892832270723,1.,1.32828000610448));
#28967=CARTESIAN_POINT('Ctrl Pts',(-1.61284234015762,1.,1.32683074483365));
#28968=CARTESIAN_POINT('Ctrl Pts',(-1.6067775829097,1.,1.32534250785794));
#28969=CARTESIAN_POINT('Ctrl Pts',(-1.600735118587,1.,1.32381550858266));
#28970=CARTESIAN_POINT('Ctrl Pts',(-1.59471591079408,1.,1.32224985747686));
#28971=CARTESIAN_POINT('Ctrl Pts',(-1.58872057258244,1.,1.32064537110891));
#28972=CARTESIAN_POINT('Ctrl Pts',(-1.58274907898829,1.,1.31900135021428));
#28973=CARTESIAN_POINT('Ctrl Pts',(-1.57680056505585,1.,1.31731642317183));
#28974=CARTESIAN_POINT('Ctrl Pts',(-1.57087397835721,1.,1.31558903860015));
#28975=CARTESIAN_POINT('Ctrl Pts',(-1.56496872402352,1.,1.31381795281002));
#28976=CARTESIAN_POINT('Ctrl Pts',(-1.55908521254822,1.,1.31200264341696));
#28977=CARTESIAN_POINT('Ctrl Pts',(-1.55322568759481,1.,1.31014393684221));
#28978=CARTESIAN_POINT('Ctrl Pts',(-1.54739413957183,1.,1.30824393907471));
#28979=CARTESIAN_POINT('Ctrl Pts',(-1.54159462645428,1.,1.30630475189553));
#28980=CARTESIAN_POINT('Ctrl Pts',(-1.53582981268976,1.,1.30432735639487));
#28981=CARTESIAN_POINT('Ctrl Pts',(-1.53009970283893,1.,1.3023106439557));
#28982=CARTESIAN_POINT('Ctrl Pts',(-1.5243995786107,1.,1.30024984366334));
#28983=CARTESIAN_POINT('Ctrl Pts',(-1.51872184912735,1.,1.29813791800757));
#28984=CARTESIAN_POINT('Ctrl Pts',(-1.51305994241412,1.,1.29596850710518));
#28985=CARTESIAN_POINT('Ctrl Pts',(-1.50741159078367,1.,1.29373841372843));
#28986=CARTESIAN_POINT('Ctrl Pts',(-1.50178230149764,1.,1.29145022885171));
#28987=CARTESIAN_POINT('Ctrl Pts',(-1.49618896881729,1.,1.28911506584232));
#28988=CARTESIAN_POINT('Ctrl Pts',(-1.4906522831275,1.,1.28674676116415));
#28989=CARTESIAN_POINT('Ctrl Pts',(-1.48518817118891,1.,1.28435533880184));
#28990=CARTESIAN_POINT('Ctrl Pts',(-1.47980070347102,1.,1.28194158939522));
#28991=CARTESIAN_POINT('Ctrl Pts',(-1.4744717526711,1.,1.27948918248524));
#28992=CARTESIAN_POINT('Ctrl Pts',(-1.46916035917197,1.,1.27696414831144));
#28993=CARTESIAN_POINT('Ctrl Pts',(-1.4638243133254,1.,1.27433119897877));
#28994=CARTESIAN_POINT('Ctrl Pts',(-1.45843906294725,1.,1.27156805265312));
#28995=CARTESIAN_POINT('Ctrl Pts',(-1.45301422764205,1.,1.26867786804854));
#28996=CARTESIAN_POINT('Ctrl Pts',(-1.44761985001544,1.,1.26570925118767));
#28997=CARTESIAN_POINT('Ctrl Pts',(-1.44236470511145,1.,1.26273903323723));
#28998=CARTESIAN_POINT('Ctrl Pts',(-1.43734919180719,1.,1.25983531011894));
#28999=CARTESIAN_POINT('Ctrl Pts',(-1.43262645609679,1.,1.25702687965744));
#29000=CARTESIAN_POINT('Ctrl Pts',(-1.42815938799555,1.,1.25426945222783));
#29001=CARTESIAN_POINT('Ctrl Pts',(-1.42378102115911,1.,1.25141455570299));
#29002=CARTESIAN_POINT('Ctrl Pts',(-1.41923722596421,1.,1.24824430986911));
#29003=CARTESIAN_POINT('Ctrl Pts',(-1.41422913175437,1.,1.24450600513278));
#29004=CARTESIAN_POINT('Ctrl Pts',(-1.40845295531151,1.,1.23994455029421));
#29005=CARTESIAN_POINT('Ctrl Pts',(-1.40164708205345,1.,1.23434087289768));
#29006=CARTESIAN_POINT('Ctrl Pts',(-1.39361389567257,1.,1.22752961898063));
#29007=CARTESIAN_POINT('Ctrl Pts',(-1.38420564525391,1.,1.21938737278853));
#29008=CARTESIAN_POINT('Ctrl Pts',(-1.37331915604962,1.,1.20982812923113));
#29009=CARTESIAN_POINT('Ctrl Pts',(-1.36088705040677,1.,1.1987959077656));
#29010=CARTESIAN_POINT('Ctrl Pts',(-1.34687053998157,1.,1.18625865664915));
#29011=CARTESIAN_POINT('Ctrl Pts',(-1.33437539344842,1.,1.17501305787994));
#29012=CARTESIAN_POINT('Ctrl Pts',(-1.32428080720544,1.,1.16589330092532));
#29013=CARTESIAN_POINT('Ctrl Pts',(-1.3172297721596,1.,1.15950888730433));
#29014=CARTESIAN_POINT('Ctrl Pts',(-1.31362392696033,1.,1.15624053661742));
#29015=CARTESIAN_POINT('',(-1.73811241238545,0.,1.34869019493419));
#29016=CARTESIAN_POINT('Origin',(-1.81978687191668,0.,1.23627494547115));
#29017=CARTESIAN_POINT('',(-1.81978687191668,1.,1.23627494547115));
#29018=CARTESIAN_POINT('',(-1.73811241238545,1.,1.34869019493419));
#29019=CARTESIAN_POINT('',(-1.81978687191668,0.,1.23627494547115));
#29020=CARTESIAN_POINT('Ctrl Pts',(-1.5055822144029,-1.,0.892032620296855));
#29021=CARTESIAN_POINT('Ctrl Pts',(-1.5055822144029,1.,0.892032620296855));
#29022=CARTESIAN_POINT('Ctrl Pts',(-1.50980486807181,-1.,0.894452006967538));
#29023=CARTESIAN_POINT('Ctrl Pts',(-1.50980486807181,1.,0.894452006967538));
#29024=CARTESIAN_POINT('Ctrl Pts',(-1.51805569591479,-1.,0.89918504749193));
#29025=CARTESIAN_POINT('Ctrl Pts',(-1.51805569591479,1.,0.89918504749193));
#29026=CARTESIAN_POINT('Ctrl Pts',(-1.52984849890434,-1.,0.905967409640499));
#29027=CARTESIAN_POINT('Ctrl Pts',(-1.52984849890434,1.,0.905967409640499));
#29028=CARTESIAN_POINT('Ctrl Pts',(-1.54440491152808,-1.,0.91437591904658));
#29029=CARTESIAN_POINT('Ctrl Pts',(-1.54440491152808,1.,0.91437591904658));
#29030=CARTESIAN_POINT('Ctrl Pts',(-1.56065988582509,-1.,0.923832188966322));
#29031=CARTESIAN_POINT('Ctrl Pts',(-1.56065988582509,1.,0.923832188966322));
#29032=CARTESIAN_POINT('Ctrl Pts',(-1.57499388385561,-1.,0.932246680128849));
#29033=CARTESIAN_POINT('Ctrl Pts',(-1.57499388385561,1.,0.932246680128849));
#29034=CARTESIAN_POINT('Ctrl Pts',(-1.58744937489796,-1.,0.939646377909319));
#29035=CARTESIAN_POINT('Ctrl Pts',(-1.58744937489796,1.,0.939646377909319));
#29036=CARTESIAN_POINT('Ctrl Pts',(-1.59810042045408,-1.,0.946078063325796));
#29037=CARTESIAN_POINT('Ctrl Pts',(-1.59810042045408,1.,0.946078063325796));
#29038=CARTESIAN_POINT('Ctrl Pts',(-1.60706069897794,-1.,0.951613284361248));
#29039=CARTESIAN_POINT('Ctrl Pts',(-1.60706069897794,1.,0.951613284361248));
#29040=CARTESIAN_POINT('Ctrl Pts',(-1.61449324337233,-1.,0.956354422921573));
#29041=CARTESIAN_POINT('Ctrl Pts',(-1.61449324337233,1.,0.956354422921573));
#29042=CARTESIAN_POINT('Ctrl Pts',(-1.62061638139929,-1.,0.960438326099958));
#29043=CARTESIAN_POINT('Ctrl Pts',(-1.62061638139929,1.,0.960438326099958));
#29044=CARTESIAN_POINT('Ctrl Pts',(-1.6257193066974,-1.,0.964046107037821));
#29045=CARTESIAN_POINT('Ctrl Pts',(-1.6257193066974,1.,0.964046107037821));
#29046=CARTESIAN_POINT('Ctrl Pts',(-1.63013849959083,-1.,0.967387853228041));
#29047=CARTESIAN_POINT('Ctrl Pts',(-1.63013849959083,1.,0.967387853228041));
#29048=CARTESIAN_POINT('Ctrl Pts',(-1.63420665729609,-1.,0.970669715996356));
#29049=CARTESIAN_POINT('Ctrl Pts',(-1.63420665729609,1.,0.970669715996356));
#29050=CARTESIAN_POINT('Ctrl Pts',(-1.63820952658157,-1.,0.974066058287501));
#29051=CARTESIAN_POINT('Ctrl Pts',(-1.63820952658157,1.,0.974066058287501));
#29052=CARTESIAN_POINT('Ctrl Pts',(-1.64233990826831,-1.,0.977689794120297));
#29053=CARTESIAN_POINT('Ctrl Pts',(-1.64233990826831,1.,0.977689794120297));
#29054=CARTESIAN_POINT('Ctrl Pts',(-1.64665139190834,-1.,0.981562530940574));
#29055=CARTESIAN_POINT('Ctrl Pts',(-1.64665139190834,1.,0.981562530940574));
#29056=CARTESIAN_POINT('Ctrl Pts',(-1.6511001661277,-1.,0.985642622921626));
#29057=CARTESIAN_POINT('Ctrl Pts',(-1.6511001661277,1.,0.985642622921626));
#29058=CARTESIAN_POINT('Ctrl Pts',(-1.65559044289746,-1.,0.98985562785445));
#29059=CARTESIAN_POINT('Ctrl Pts',(-1.65559044289746,1.,0.98985562785445));
#29060=CARTESIAN_POINT('Ctrl Pts',(-1.66001553809916,-1.,0.994121836661116));
#29061=CARTESIAN_POINT('Ctrl Pts',(-1.66001553809916,1.,0.994121836661116));
#29062=CARTESIAN_POINT('Ctrl Pts',(-1.66430758030304,-1.,0.998389654952317));
#29063=CARTESIAN_POINT('Ctrl Pts',(-1.66430758030304,1.,0.998389654952317));
#29064=CARTESIAN_POINT('Ctrl Pts',(-1.66846059277231,-1.,1.00265091003682));
#29065=CARTESIAN_POINT('Ctrl Pts',(-1.66846059277231,1.,1.00265091003682));
#29066=CARTESIAN_POINT('Ctrl Pts',(-1.67250335383248,-1.,1.00692206696387));
#29067=CARTESIAN_POINT('Ctrl Pts',(-1.67250335383248,1.,1.00692206696387));
#29068=CARTESIAN_POINT('Ctrl Pts',(-1.67648246776457,-1.,1.01123236493507));
#29069=CARTESIAN_POINT('Ctrl Pts',(-1.67648246776457,1.,1.01123236493507));
#29070=CARTESIAN_POINT('Ctrl Pts',(-1.6804428989482,-1.,1.01561026162787));
#29071=CARTESIAN_POINT('Ctrl Pts',(-1.6804428989482,1.,1.01561026162787));
#29072=CARTESIAN_POINT('Ctrl Pts',(-1.68440578021739,-1.,1.02006795074222));
#29073=CARTESIAN_POINT('Ctrl Pts',(-1.68440578021739,1.,1.02006795074222));
#29074=CARTESIAN_POINT('Ctrl Pts',(-1.68836910178475,-1.,1.02460180535272));
#29075=CARTESIAN_POINT('Ctrl Pts',(-1.68836910178475,1.,1.02460180535272));
#29076=CARTESIAN_POINT('Ctrl Pts',(-1.69231840863471,-1.,1.02919977579155));
#29077=CARTESIAN_POINT('Ctrl Pts',(-1.69231840863471,1.,1.02919977579155));
#29078=CARTESIAN_POINT('Ctrl Pts',(-1.69623414782769,-1.,1.03384646003587));
#29079=CARTESIAN_POINT('Ctrl Pts',(-1.69623414782769,1.,1.03384646003587));
#29080=CARTESIAN_POINT('Ctrl Pts',(-1.70010052930951,-1.,1.03852922490782));
#29081=CARTESIAN_POINT('Ctrl Pts',(-1.70010052930951,1.,1.03852922490782));
#29082=CARTESIAN_POINT('Ctrl Pts',(-1.70391338707969,-1.,1.04324363334546));
#29083=CARTESIAN_POINT('Ctrl Pts',(-1.70391338707969,1.,1.04324363334546));
#29084=CARTESIAN_POINT('Ctrl Pts',(-1.70767646263641,-1.,1.0479908540499));
#29085=CARTESIAN_POINT('Ctrl Pts',(-1.70767646263641,1.,1.0479908540499));
#29086=CARTESIAN_POINT('Ctrl Pts',(-1.71139783543986,-1.,1.05277517202854));
#29087=CARTESIAN_POINT('Ctrl Pts',(-1.71139783543986,1.,1.05277517202854));
#29088=CARTESIAN_POINT('Ctrl Pts',(-1.71508654427022,-1.,1.05760163192481));
#29089=CARTESIAN_POINT('Ctrl Pts',(-1.71508654427022,1.,1.05760163192481));
#29090=CARTESIAN_POINT('Ctrl Pts',(-1.71874858456908,-1.,1.0624732468065));
#29091=CARTESIAN_POINT('Ctrl Pts',(-1.71874858456908,1.,1.0624732468065));
#29092=CARTESIAN_POINT('Ctrl Pts',(-1.72238500928456,-1.,1.06738966975463));
#29093=CARTESIAN_POINT('Ctrl Pts',(-1.72238500928456,1.,1.06738966975463));
#29094=CARTESIAN_POINT('Ctrl Pts',(-1.72599406198489,-1.,1.07234866990252));
#29095=CARTESIAN_POINT('Ctrl Pts',(-1.72599406198489,1.,1.07234866990252));
#29096=CARTESIAN_POINT('Ctrl Pts',(-1.72957248977424,-1.,1.0773470373727));
#29097=CARTESIAN_POINT('Ctrl Pts',(-1.72957248977424,1.,1.0773470373727));
#29098=CARTESIAN_POINT('Ctrl Pts',(-1.73311705663407,-1.,1.08238162784749));
#29099=CARTESIAN_POINT('Ctrl Pts',(-1.73311705663407,1.,1.08238162784749));
#29100=CARTESIAN_POINT('Ctrl Pts',(-1.73662628326093,-1.,1.08745056285429));
#29101=CARTESIAN_POINT('Ctrl Pts',(-1.73662628326093,1.,1.08745056285429));
#29102=CARTESIAN_POINT('Ctrl Pts',(-1.74010053962252,-1.,1.09255329056496));
#29103=CARTESIAN_POINT('Ctrl Pts',(-1.74010053962252,1.,1.09255329056496));
#29104=CARTESIAN_POINT('Ctrl Pts',(-1.74354119236212,-1.,1.09768999241229));
#29105=CARTESIAN_POINT('Ctrl Pts',(-1.74354119236212,1.,1.09768999241229));
#29106=CARTESIAN_POINT('Ctrl Pts',(-1.74695004214924,-1.,1.10286118991144));
#29107=CARTESIAN_POINT('Ctrl Pts',(-1.74695004214924,1.,1.10286118991144));
#29108=CARTESIAN_POINT('Ctrl Pts',(-1.75032866075914,-1.,1.10806728183003));
#29109=CARTESIAN_POINT('Ctrl Pts',(-1.75032866075914,1.,1.10806728183003));
#29110=CARTESIAN_POINT('Ctrl Pts',(-1.75367772094617,-1.,1.11330807582542));
#29111=CARTESIAN_POINT('Ctrl Pts',(-1.75367772094617,1.,1.11330807582542));
#29112=CARTESIAN_POINT('Ctrl Pts',(-1.75699720772089,-1.,1.11858293216752));
#29113=CARTESIAN_POINT('Ctrl Pts',(-1.75699720772089,1.,1.11858293216752));
#29114=CARTESIAN_POINT('Ctrl Pts',(-1.76028671825084,-1.,1.12389096855078));
#29115=CARTESIAN_POINT('Ctrl Pts',(-1.76028671825084,1.,1.12389096855078));
#29116=CARTESIAN_POINT('Ctrl Pts',(-1.76354571966171,-1.,1.12923123555076));
#29117=CARTESIAN_POINT('Ctrl Pts',(-1.76354571966171,1.,1.12923123555076));
#29118=CARTESIAN_POINT('Ctrl Pts',(-1.76677384551883,-1.,1.13460291804635));
#29119=CARTESIAN_POINT('Ctrl Pts',(-1.76677384551883,1.,1.13460291804635));
#29120=CARTESIAN_POINT('Ctrl Pts',(-1.76997111386806,-1.,1.14000548337));
#29121=CARTESIAN_POINT('Ctrl Pts',(-1.76997111386806,1.,1.14000548337));
#29122=CARTESIAN_POINT('Ctrl Pts',(-1.77313777896234,-1.,1.14543858226948));
#29123=CARTESIAN_POINT('Ctrl Pts',(-1.77313777896234,1.,1.14543858226948));
#29124=CARTESIAN_POINT('Ctrl Pts',(-1.77627422557034,-1.,1.15090197841531));
#29125=CARTESIAN_POINT('Ctrl Pts',(-1.77627422557034,1.,1.15090197841531));
#29126=CARTESIAN_POINT('Ctrl Pts',(-1.77938085564261,-1.,1.15639547194689));
#29127=CARTESIAN_POINT('Ctrl Pts',(-1.77938085564261,1.,1.15639547194689));
#29128=CARTESIAN_POINT('Ctrl Pts',(-1.78245795880949,-1.,1.16191881298458));
#29129=CARTESIAN_POINT('Ctrl Pts',(-1.78245795880949,1.,1.16191881298458));
#29130=CARTESIAN_POINT('Ctrl Pts',(-1.78550566040349,-1.,1.16747166312239));
#29131=CARTESIAN_POINT('Ctrl Pts',(-1.78550566040349,1.,1.16747166312239));
#29132=CARTESIAN_POINT('Ctrl Pts',(-1.78852398877523,-1.,1.17305363177265));
#29133=CARTESIAN_POINT('Ctrl Pts',(-1.78852398877523,1.,1.17305363177265));
#29134=CARTESIAN_POINT('Ctrl Pts',(-1.79151291552646,-1.,1.17866429440781));
#29135=CARTESIAN_POINT('Ctrl Pts',(-1.79151291552646,1.,1.17866429440781));
#29136=CARTESIAN_POINT('Ctrl Pts',(-1.79447240321572,-1.,1.18430321697471));
#29137=CARTESIAN_POINT('Ctrl Pts',(-1.79447240321572,1.,1.18430321697471));
#29138=CARTESIAN_POINT('Ctrl Pts',(-1.79740245923649,-1.,1.1899699793456));
#29139=CARTESIAN_POINT('Ctrl Pts',(-1.79740245923649,1.,1.1899699793456));
#29140=CARTESIAN_POINT('Ctrl Pts',(-1.80030314370121,-1.,1.19566418930405));
#29141=CARTESIAN_POINT('Ctrl Pts',(-1.80030314370121,1.,1.19566418930405));
#29142=CARTESIAN_POINT('Ctrl Pts',(-1.8031745483882,-1.,1.2013854893912));
#29143=CARTESIAN_POINT('Ctrl Pts',(-1.8031745483882,1.,1.2013854893912));
#29144=CARTESIAN_POINT('Ctrl Pts',(-1.80601678480772,-1.,1.20713356605519));
#29145=CARTESIAN_POINT('Ctrl Pts',(-1.80601678480772,1.,1.20713356605519));
#29146=CARTESIAN_POINT('Ctrl Pts',(-1.80882996916931,-1.,1.2129081570818));
#29147=CARTESIAN_POINT('Ctrl Pts',(-1.80882996916931,1.,1.2129081570818));
#29148=CARTESIAN_POINT('Ctrl Pts',(-1.81161420806172,-1.,1.2187090610323));
#29149=CARTESIAN_POINT('Ctrl Pts',(-1.81161420806172,1.,1.2187090610323));
#29150=CARTESIAN_POINT('Ctrl Pts',(-1.81436959209778,-1.,1.22453613304507));
#29151=CARTESIAN_POINT('Ctrl Pts',(-1.81436959209778,1.,1.22453613304507));
#29152=CARTESIAN_POINT('Ctrl Pts',(-1.81655087183054,-1.,1.22921864890975));
#29153=CARTESIAN_POINT('Ctrl Pts',(-1.81655087183054,1.,1.22921864890975));
#29154=CARTESIAN_POINT('Ctrl Pts',(-1.81817389920914,-1.,1.23274224526804));
#29155=CARTESIAN_POINT('Ctrl Pts',(-1.81817389920914,1.,1.23274224526804));
#29156=CARTESIAN_POINT('Ctrl Pts',(-1.81925017193531,-1.,1.23509651170384));
#29157=CARTESIAN_POINT('Ctrl Pts',(-1.81925017193531,1.,1.23509651170384));
#29158=CARTESIAN_POINT('Ctrl Pts',(-1.81978687191668,-1.,1.23627494547115));
#29159=CARTESIAN_POINT('Ctrl Pts',(-1.81978687191668,1.,1.23627494547115));
#29160=CARTESIAN_POINT('',(-1.5055822144029,1.,0.892032620296855));
#29161=CARTESIAN_POINT('Ctrl Pts',(-1.5055822144029,1.,0.892032620296855));
#29162=CARTESIAN_POINT('Ctrl Pts',(-1.50980486807181,1.,0.894452006967538));
#29163=CARTESIAN_POINT('Ctrl Pts',(-1.51805569591479,1.,0.89918504749193));
#29164=CARTESIAN_POINT('Ctrl Pts',(-1.52984849890434,1.,0.905967409640499));
#29165=CARTESIAN_POINT('Ctrl Pts',(-1.54440491152808,1.,0.91437591904658));
#29166=CARTESIAN_POINT('Ctrl Pts',(-1.56065988582509,1.,0.923832188966322));
#29167=CARTESIAN_POINT('Ctrl Pts',(-1.57499388385561,1.,0.932246680128849));
#29168=CARTESIAN_POINT('Ctrl Pts',(-1.58744937489796,1.,0.939646377909319));
#29169=CARTESIAN_POINT('Ctrl Pts',(-1.59810042045408,1.,0.946078063325796));
#29170=CARTESIAN_POINT('Ctrl Pts',(-1.60706069897794,1.,0.951613284361248));
#29171=CARTESIAN_POINT('Ctrl Pts',(-1.61449324337233,1.,0.956354422921573));
#29172=CARTESIAN_POINT('Ctrl Pts',(-1.62061638139929,1.,0.960438326099958));
#29173=CARTESIAN_POINT('Ctrl Pts',(-1.6257193066974,1.,0.964046107037821));
#29174=CARTESIAN_POINT('Ctrl Pts',(-1.63013849959083,1.,0.967387853228041));
#29175=CARTESIAN_POINT('Ctrl Pts',(-1.63420665729609,1.,0.970669715996356));
#29176=CARTESIAN_POINT('Ctrl Pts',(-1.63820952658157,1.,0.974066058287501));
#29177=CARTESIAN_POINT('Ctrl Pts',(-1.64233990826831,1.,0.977689794120297));
#29178=CARTESIAN_POINT('Ctrl Pts',(-1.64665139190834,1.,0.981562530940574));
#29179=CARTESIAN_POINT('Ctrl Pts',(-1.6511001661277,1.,0.985642622921626));
#29180=CARTESIAN_POINT('Ctrl Pts',(-1.65559044289746,1.,0.98985562785445));
#29181=CARTESIAN_POINT('Ctrl Pts',(-1.66001553809916,1.,0.994121836661116));
#29182=CARTESIAN_POINT('Ctrl Pts',(-1.66430758030304,1.,0.998389654952317));
#29183=CARTESIAN_POINT('Ctrl Pts',(-1.66846059277231,1.,1.00265091003682));
#29184=CARTESIAN_POINT('Ctrl Pts',(-1.67250335383248,1.,1.00692206696387));
#29185=CARTESIAN_POINT('Ctrl Pts',(-1.67648246776457,1.,1.01123236493507));
#29186=CARTESIAN_POINT('Ctrl Pts',(-1.6804428989482,1.,1.01561026162787));
#29187=CARTESIAN_POINT('Ctrl Pts',(-1.68440578021739,1.,1.02006795074222));
#29188=CARTESIAN_POINT('Ctrl Pts',(-1.68836910178475,1.,1.02460180535272));
#29189=CARTESIAN_POINT('Ctrl Pts',(-1.69231840863471,1.,1.02919977579155));
#29190=CARTESIAN_POINT('Ctrl Pts',(-1.69623414782769,1.,1.03384646003587));
#29191=CARTESIAN_POINT('Ctrl Pts',(-1.70010052930951,1.,1.03852922490782));
#29192=CARTESIAN_POINT('Ctrl Pts',(-1.70391338707969,1.,1.04324363334546));
#29193=CARTESIAN_POINT('Ctrl Pts',(-1.70767646263641,1.,1.0479908540499));
#29194=CARTESIAN_POINT('Ctrl Pts',(-1.71139783543986,1.,1.05277517202854));
#29195=CARTESIAN_POINT('Ctrl Pts',(-1.71508654427022,1.,1.05760163192481));
#29196=CARTESIAN_POINT('Ctrl Pts',(-1.71874858456908,1.,1.0624732468065));
#29197=CARTESIAN_POINT('Ctrl Pts',(-1.72238500928456,1.,1.06738966975463));
#29198=CARTESIAN_POINT('Ctrl Pts',(-1.72599406198489,1.,1.07234866990252));
#29199=CARTESIAN_POINT('Ctrl Pts',(-1.72957248977424,1.,1.0773470373727));
#29200=CARTESIAN_POINT('Ctrl Pts',(-1.73311705663407,1.,1.08238162784749));
#29201=CARTESIAN_POINT('Ctrl Pts',(-1.73662628326093,1.,1.08745056285429));
#29202=CARTESIAN_POINT('Ctrl Pts',(-1.74010053962252,1.,1.09255329056496));
#29203=CARTESIAN_POINT('Ctrl Pts',(-1.74354119236212,1.,1.09768999241229));
#29204=CARTESIAN_POINT('Ctrl Pts',(-1.74695004214924,1.,1.10286118991144));
#29205=CARTESIAN_POINT('Ctrl Pts',(-1.75032866075914,1.,1.10806728183003));
#29206=CARTESIAN_POINT('Ctrl Pts',(-1.75367772094617,1.,1.11330807582542));
#29207=CARTESIAN_POINT('Ctrl Pts',(-1.75699720772089,1.,1.11858293216752));
#29208=CARTESIAN_POINT('Ctrl Pts',(-1.76028671825084,1.,1.12389096855078));
#29209=CARTESIAN_POINT('Ctrl Pts',(-1.76354571966171,1.,1.12923123555076));
#29210=CARTESIAN_POINT('Ctrl Pts',(-1.76677384551883,1.,1.13460291804635));
#29211=CARTESIAN_POINT('Ctrl Pts',(-1.76997111386806,1.,1.14000548337));
#29212=CARTESIAN_POINT('Ctrl Pts',(-1.77313777896234,1.,1.14543858226948));
#29213=CARTESIAN_POINT('Ctrl Pts',(-1.77627422557034,1.,1.15090197841531));
#29214=CARTESIAN_POINT('Ctrl Pts',(-1.77938085564261,1.,1.15639547194689));
#29215=CARTESIAN_POINT('Ctrl Pts',(-1.78245795880949,1.,1.16191881298458));
#29216=CARTESIAN_POINT('Ctrl Pts',(-1.78550566040349,1.,1.16747166312239));
#29217=CARTESIAN_POINT('Ctrl Pts',(-1.78852398877523,1.,1.17305363177265));
#29218=CARTESIAN_POINT('Ctrl Pts',(-1.79151291552646,1.,1.17866429440781));
#29219=CARTESIAN_POINT('Ctrl Pts',(-1.79447240321572,1.,1.18430321697471));
#29220=CARTESIAN_POINT('Ctrl Pts',(-1.79740245923649,1.,1.1899699793456));
#29221=CARTESIAN_POINT('Ctrl Pts',(-1.80030314370121,1.,1.19566418930405));
#29222=CARTESIAN_POINT('Ctrl Pts',(-1.8031745483882,1.,1.2013854893912));
#29223=CARTESIAN_POINT('Ctrl Pts',(-1.80601678480772,1.,1.20713356605519));
#29224=CARTESIAN_POINT('Ctrl Pts',(-1.80882996916931,1.,1.2129081570818));
#29225=CARTESIAN_POINT('Ctrl Pts',(-1.81161420806172,1.,1.2187090610323));
#29226=CARTESIAN_POINT('Ctrl Pts',(-1.81436959209778,1.,1.22453613304507));
#29227=CARTESIAN_POINT('Ctrl Pts',(-1.81655087183054,1.,1.22921864890975));
#29228=CARTESIAN_POINT('Ctrl Pts',(-1.81817389920914,1.,1.23274224526804));
#29229=CARTESIAN_POINT('Ctrl Pts',(-1.81925017193531,1.,1.23509651170384));
#29230=CARTESIAN_POINT('Ctrl Pts',(-1.81978687191668,1.,1.23627494547115));
#29231=CARTESIAN_POINT('',(-1.5055822144029,0.,0.892032620296856));
#29232=CARTESIAN_POINT('Origin',(0.,0.,0.));
#29233=CARTESIAN_POINT('',(-1.60662857109684,1.,0.693717979106305));
#29234=CARTESIAN_POINT('Origin',(0.,1.,0.));
#29235=CARTESIAN_POINT('',(-1.60662857109684,0.,0.693717979106306));
#29236=CARTESIAN_POINT('Ctrl Pts',(-2.0698113262342,-1.,0.7455743247944));
#29237=CARTESIAN_POINT('Ctrl Pts',(-2.0698113262342,1.,0.7455743247944));
#29238=CARTESIAN_POINT('Ctrl Pts',(-2.06854248895728,-1.,0.745832791378367));
#29239=CARTESIAN_POINT('Ctrl Pts',(-2.06854248895728,1.,0.745832791378367));
#29240=CARTESIAN_POINT('Ctrl Pts',(-2.06600523016815,-1.,0.7463458715442));
#29241=CARTESIAN_POINT('Ctrl Pts',(-2.06600523016815,1.,0.7463458715442));
#29242=CARTESIAN_POINT('Ctrl Pts',(-2.06220058927826,-1.,0.747103932787919));
#29243=CARTESIAN_POINT('Ctrl Pts',(-2.06220058927826,1.,0.747103932787919));
#29244=CARTESIAN_POINT('Ctrl Pts',(-2.05713023031006,-1.,0.748091554183802));
#29245=CARTESIAN_POINT('Ctrl Pts',(-2.05713023031006,1.,0.748091554183802));
#29246=CARTESIAN_POINT('Ctrl Pts',(-2.05079645592154,-1.,0.749287468665046));
#29247=CARTESIAN_POINT('Ctrl Pts',(-2.05079645592154,1.,0.749287468665046));
#29248=CARTESIAN_POINT('Ctrl Pts',(-2.04446689147979,-1.,0.750444657875576));
#29249=CARTESIAN_POINT('Ctrl Pts',(-2.04446689147979,1.,0.750444657875576));
#29250=CARTESIAN_POINT('Ctrl Pts',(-2.03814160092099,-1.,0.751562963361115));
#29251=CARTESIAN_POINT('Ctrl Pts',(-2.03814160092099,1.,0.751562963361115));
#29252=CARTESIAN_POINT('Ctrl Pts',(-2.03182068456221,-1.,0.752642180487211));
#29253=CARTESIAN_POINT('Ctrl Pts',(-2.03182068456221,1.,0.752642180487211));
#29254=CARTESIAN_POINT('Ctrl Pts',(-2.02550428623313,-1.,0.753682061112768));
#29255=CARTESIAN_POINT('Ctrl Pts',(-2.02550428623313,1.,0.753682061112768));
#29256=CARTESIAN_POINT('Ctrl Pts',(-2.01919259405809,-1.,0.754682330722816));
#29257=CARTESIAN_POINT('Ctrl Pts',(-2.01919259405809,1.,0.754682330722816));
#29258=CARTESIAN_POINT('Ctrl Pts',(-2.01288584328084,-1.,0.755642704957865));
#29259=CARTESIAN_POINT('Ctrl Pts',(-2.01288584328084,1.,0.755642704957865));
#29260=CARTESIAN_POINT('Ctrl Pts',(-2.0065843158773,-1.,0.75656290464667));
#29261=CARTESIAN_POINT('Ctrl Pts',(-2.0065843158773,1.,0.75656290464667));
#29262=CARTESIAN_POINT('Ctrl Pts',(-2.00028834739178,-1.,0.757442676862724));
#29263=CARTESIAN_POINT('Ctrl Pts',(-2.00028834739178,1.,0.757442676862724));
#29264=CARTESIAN_POINT('Ctrl Pts',(-1.99399831098817,-1.,0.758281796766761));
#29265=CARTESIAN_POINT('Ctrl Pts',(-1.99399831098817,1.,0.758281796766761));
#29266=CARTESIAN_POINT('Ctrl Pts',(-1.98771456680874,-1.,0.759080037802488));
#29267=CARTESIAN_POINT('Ctrl Pts',(-1.98771456680874,1.,0.759080037802488));
#29268=CARTESIAN_POINT('Ctrl Pts',(-1.98143741418172,-1.,0.75983714745219));
#29269=CARTESIAN_POINT('Ctrl Pts',(-1.98143741418172,1.,0.75983714745219));
#29270=CARTESIAN_POINT('Ctrl Pts',(-1.97516705321494,-1.,0.760552825409757));
#29271=CARTESIAN_POINT('Ctrl Pts',(-1.97516705321494,1.,0.760552825409757));
#29272=CARTESIAN_POINT('Ctrl Pts',(-1.96890351582499,-1.,0.76122669048382));
#29273=CARTESIAN_POINT('Ctrl Pts',(-1.96890351582499,1.,0.76122669048382));
#29274=CARTESIAN_POINT('Ctrl Pts',(-1.96264672744186,-1.,0.761858300014423));
#29275=CARTESIAN_POINT('Ctrl Pts',(-1.96264672744186,1.,0.761858300014423));
#29276=CARTESIAN_POINT('Ctrl Pts',(-1.95639665309869,-1.,0.762447203806179));
#29277=CARTESIAN_POINT('Ctrl Pts',(-1.95639665309869,1.,0.762447203806179));
#29278=CARTESIAN_POINT('Ctrl Pts',(-1.95015342590024,-1.,0.762992990878769));
#29279=CARTESIAN_POINT('Ctrl Pts',(-1.95015342590024,1.,0.762992990878769));
#29280=CARTESIAN_POINT('Ctrl Pts',(-1.9439174661764,-1.,0.763495333538629));
#29281=CARTESIAN_POINT('Ctrl Pts',(-1.9439174661764,1.,0.763495333538629));
#29282=CARTESIAN_POINT('Ctrl Pts',(-1.93768964875886,-1.,0.763954049121458));
#29283=CARTESIAN_POINT('Ctrl Pts',(-1.93768964875886,1.,0.763954049121458));
#29284=CARTESIAN_POINT('Ctrl Pts',(-1.93147105496382,-1.,0.76436901067394));
#29285=CARTESIAN_POINT('Ctrl Pts',(-1.93147105496382,1.,0.76436901067394));
#29286=CARTESIAN_POINT('Ctrl Pts',(-1.92526263537048,-1.,0.764740025488211));
#29287=CARTESIAN_POINT('Ctrl Pts',(-1.92526263537048,1.,0.764740025488211));
#29288=CARTESIAN_POINT('Ctrl Pts',(-1.91906491634196,-1.,0.765066729667088));
#29289=CARTESIAN_POINT('Ctrl Pts',(-1.91906491634196,1.,0.765066729667088));
#29290=CARTESIAN_POINT('Ctrl Pts',(-1.91287765805169,-1.,0.765348465884722));
#29291=CARTESIAN_POINT('Ctrl Pts',(-1.91287765805169,1.,0.765348465884722));
#29292=CARTESIAN_POINT('Ctrl Pts',(-1.90669961402356,-1.,0.765584196937919));
#29293=CARTESIAN_POINT('Ctrl Pts',(-1.90669961402356,1.,0.765584196937919));
#29294=CARTESIAN_POINT('Ctrl Pts',(-1.90052930393596,-1.,0.765772772593386));
#29295=CARTESIAN_POINT('Ctrl Pts',(-1.90052930393596,1.,0.765772772593386));
#29296=CARTESIAN_POINT('Ctrl Pts',(-1.89436577771388,-1.,0.765913193856978));
#29297=CARTESIAN_POINT('Ctrl Pts',(-1.89436577771388,1.,0.765913193856978));
#29298=CARTESIAN_POINT('Ctrl Pts',(-1.88820926433409,-1.,0.766004837062091));
#29299=CARTESIAN_POINT('Ctrl Pts',(-1.88820926433409,1.,0.766004837062091));
#29300=CARTESIAN_POINT('Ctrl Pts',(-1.88206215302561,-1.,0.766047794851864));
#29301=CARTESIAN_POINT('Ctrl Pts',(-1.88206215302561,1.,0.766047794851864));
#29302=CARTESIAN_POINT('Ctrl Pts',(-1.87592888967883,-1.,0.766042837036744));
#29303=CARTESIAN_POINT('Ctrl Pts',(-1.87592888967883,1.,0.766042837036744));
#29304=CARTESIAN_POINT('Ctrl Pts',(-1.86981398314341,-1.,0.765990708546091));
#29305=CARTESIAN_POINT('Ctrl Pts',(-1.86981398314341,1.,0.765990708546091));
#29306=CARTESIAN_POINT('Ctrl Pts',(-1.86372027063312,-1.,0.765891519092547));
#29307=CARTESIAN_POINT('Ctrl Pts',(-1.86372027063312,1.,0.765891519092547));
#29308=CARTESIAN_POINT('Ctrl Pts',(-1.85764741390394,-1.,0.765744212909318));
#29309=CARTESIAN_POINT('Ctrl Pts',(-1.85764741390394,1.,0.765744212909318));
#29310=CARTESIAN_POINT('Ctrl Pts',(-1.85158945130063,-1.,0.765545710619062));
#29311=CARTESIAN_POINT('Ctrl Pts',(-1.85158945130063,1.,0.765545710619062));
#29312=CARTESIAN_POINT('Ctrl Pts',(-1.84553698875924,-1.,0.765291664862029));
#29313=CARTESIAN_POINT('Ctrl Pts',(-1.84553698875924,1.,0.765291664862029));
#29314=CARTESIAN_POINT('Ctrl Pts',(-1.83948181064835,-1.,0.764978057881737));
#29315=CARTESIAN_POINT('Ctrl Pts',(-1.83948181064835,1.,0.764978057881737));
#29316=CARTESIAN_POINT('Ctrl Pts',(-1.83342077227142,-1.,0.764602549687853));
#29317=CARTESIAN_POINT('Ctrl Pts',(-1.83342077227142,1.,0.764602549687853));
#29318=CARTESIAN_POINT('Ctrl Pts',(-1.82735991200065,-1.,0.764165902605995));
#29319=CARTESIAN_POINT('Ctrl Pts',(-1.82735991200065,1.,0.764165902605995));
#29320=CARTESIAN_POINT('Ctrl Pts',(-1.82131873145266,-1.,0.763673465462726));
#29321=CARTESIAN_POINT('Ctrl Pts',(-1.82131873145266,1.,0.763673465462726));
#29322=CARTESIAN_POINT('Ctrl Pts',(-1.8153211840553,-1.,0.763132003836634));
#29323=CARTESIAN_POINT('Ctrl Pts',(-1.8153211840553,1.,0.763132003836634));
#29324=CARTESIAN_POINT('Ctrl Pts',(-1.80938551463965,-1.,0.762546129463938));
#29325=CARTESIAN_POINT('Ctrl Pts',(-1.80938551463965,1.,0.762546129463938));
#29326=CARTESIAN_POINT('Ctrl Pts',(-1.80351583877342,-1.,0.761915336443547));
#29327=CARTESIAN_POINT('Ctrl Pts',(-1.80351583877342,1.,0.761915336443547));
#29328=CARTESIAN_POINT('Ctrl Pts',(-1.79768986997783,-1.,0.761229695230558));
#29329=CARTESIAN_POINT('Ctrl Pts',(-1.79768986997783,1.,0.761229695230558));
#29330=CARTESIAN_POINT('Ctrl Pts',(-1.7918581561088,-1.,0.760469555880749));
#29331=CARTESIAN_POINT('Ctrl Pts',(-1.7918581561088,1.,0.760469555880749));
#29332=CARTESIAN_POINT('Ctrl Pts',(-1.78596964884604,-1.,0.759614401110189));
#29333=CARTESIAN_POINT('Ctrl Pts',(-1.78596964884604,1.,0.759614401110189));
#29334=CARTESIAN_POINT('Ctrl Pts',(-1.77999411220945,-1.,0.758650626677518));
#29335=CARTESIAN_POINT('Ctrl Pts',(-1.77999411220945,1.,0.758650626677518));
#29336=CARTESIAN_POINT('Ctrl Pts',(-1.77394167108292,-1.,0.757578264077029));
#29337=CARTESIAN_POINT('Ctrl Pts',(-1.77394167108292,1.,0.757578264077029));
#29338=CARTESIAN_POINT('Ctrl Pts',(-1.76789396002998,-1.,0.75642189602781));
#29339=CARTESIAN_POINT('Ctrl Pts',(-1.76789396002998,1.,0.75642189602781));
#29340=CARTESIAN_POINT('Ctrl Pts',(-1.76197817240128,-1.,0.755220979974461));
#29341=CARTESIAN_POINT('Ctrl Pts',(-1.76197817240128,1.,0.755220979974461));
#29342=CARTESIAN_POINT('Ctrl Pts',(-1.75631083600019,-1.,0.754009254027829));
#29343=CARTESIAN_POINT('Ctrl Pts',(-1.75631083600019,1.,0.754009254027829));
#29344=CARTESIAN_POINT('Ctrl Pts',(-1.75095139468794,-1.,0.752797683531314));
#29345=CARTESIAN_POINT('Ctrl Pts',(-1.75095139468794,1.,0.752797683531314));
#29346=CARTESIAN_POINT('Ctrl Pts',(-1.74585086852502,-1.,0.751555614164482));
#29347=CARTESIAN_POINT('Ctrl Pts',(-1.74585086852502,1.,0.751555614164482));
#29348=CARTESIAN_POINT('Ctrl Pts',(-1.74080458267114,-1.,0.750193435981249));
#29349=CARTESIAN_POINT('Ctrl Pts',(-1.74080458267114,1.,0.750193435981249));
#29350=CARTESIAN_POINT('Ctrl Pts',(-1.7355035168033,-1.,0.74858246295687));
#29351=CARTESIAN_POINT('Ctrl Pts',(-1.7355035168033,1.,0.74858246295687));
#29352=CARTESIAN_POINT('Ctrl Pts',(-1.72958533647714,-1.,0.746574710097752));
#29353=CARTESIAN_POINT('Ctrl Pts',(-1.72958533647714,1.,0.746574710097752));
#29354=CARTESIAN_POINT('Ctrl Pts',(-1.72268229916769,-1.,0.744021445433093));
#29355=CARTESIAN_POINT('Ctrl Pts',(-1.72268229916769,1.,0.744021445433093));
#29356=CARTESIAN_POINT('Ctrl Pts',(-1.71447789751001,-1.,0.74079516202821));
#29357=CARTESIAN_POINT('Ctrl Pts',(-1.71447789751001,1.,0.74079516202821));
#29358=CARTESIAN_POINT('Ctrl Pts',(-1.70473309004249,-1.,0.736799665716932));
#29359=CARTESIAN_POINT('Ctrl Pts',(-1.70473309004249,1.,0.736799665716932));
#29360=CARTESIAN_POINT('Ctrl Pts',(-1.69326921972915,-1.,0.731963238685357));
#29361=CARTESIAN_POINT('Ctrl Pts',(-1.69326921972915,1.,0.731963238685357));
#29362=CARTESIAN_POINT('Ctrl Pts',(-1.67996158451922,-1.,0.726235967982445));
#29363=CARTESIAN_POINT('Ctrl Pts',(-1.67996158451922,1.,0.726235967982445));
#29364=CARTESIAN_POINT('Ctrl Pts',(-1.66472880551777,-1.,0.71958543378795));
#29365=CARTESIAN_POINT('Ctrl Pts',(-1.66472880551777,1.,0.71958543378795));
#29366=CARTESIAN_POINT('Ctrl Pts',(-1.64752408828442,-1.,0.711993139340447));
#29367=CARTESIAN_POINT('Ctrl Pts',(-1.64752408828442,1.,0.711993139340447));
#29368=CARTESIAN_POINT('Ctrl Pts',(-1.6321654166204,-1.,0.705159151977294));
#29369=CARTESIAN_POINT('Ctrl Pts',(-1.6321654166204,1.,0.705159151977294));
#29370=CARTESIAN_POINT('Ctrl Pts',(-1.61974673471117,-1.,0.699605146398837));
#29371=CARTESIAN_POINT('Ctrl Pts',(-1.61974673471117,1.,0.699605146398837));
#29372=CARTESIAN_POINT('Ctrl Pts',(-1.61106790957619,-1.,0.69571209787897));
#29373=CARTESIAN_POINT('Ctrl Pts',(-1.61106790957619,1.,0.69571209787897));
#29374=CARTESIAN_POINT('Ctrl Pts',(-1.60662857109684,-1.,0.693717979106305));
#29375=CARTESIAN_POINT('Ctrl Pts',(-1.60662857109684,1.,0.693717979106305));
#29376=CARTESIAN_POINT('',(-2.0698113262342,1.,0.7455743247944));
#29377=CARTESIAN_POINT('Ctrl Pts',(-2.0698113262342,1.,0.7455743247944));
#29378=CARTESIAN_POINT('Ctrl Pts',(-2.06854248895728,1.,0.745832791378367));
#29379=CARTESIAN_POINT('Ctrl Pts',(-2.06600523016815,1.,0.7463458715442));
#29380=CARTESIAN_POINT('Ctrl Pts',(-2.06220058927826,1.,0.747103932787919));
#29381=CARTESIAN_POINT('Ctrl Pts',(-2.05713023031006,1.,0.748091554183802));
#29382=CARTESIAN_POINT('Ctrl Pts',(-2.05079645592154,1.,0.749287468665046));
#29383=CARTESIAN_POINT('Ctrl Pts',(-2.04446689147979,1.,0.750444657875576));
#29384=CARTESIAN_POINT('Ctrl Pts',(-2.03814160092099,1.,0.751562963361115));
#29385=CARTESIAN_POINT('Ctrl Pts',(-2.03182068456221,1.,0.752642180487211));
#29386=CARTESIAN_POINT('Ctrl Pts',(-2.02550428623313,1.,0.753682061112768));
#29387=CARTESIAN_POINT('Ctrl Pts',(-2.01919259405809,1.,0.754682330722816));
#29388=CARTESIAN_POINT('Ctrl Pts',(-2.01288584328084,1.,0.755642704957865));
#29389=CARTESIAN_POINT('Ctrl Pts',(-2.0065843158773,1.,0.75656290464667));
#29390=CARTESIAN_POINT('Ctrl Pts',(-2.00028834739178,1.,0.757442676862724));
#29391=CARTESIAN_POINT('Ctrl Pts',(-1.99399831098817,1.,0.758281796766761));
#29392=CARTESIAN_POINT('Ctrl Pts',(-1.98771456680874,1.,0.759080037802488));
#29393=CARTESIAN_POINT('Ctrl Pts',(-1.98143741418172,1.,0.75983714745219));
#29394=CARTESIAN_POINT('Ctrl Pts',(-1.97516705321494,1.,0.760552825409757));
#29395=CARTESIAN_POINT('Ctrl Pts',(-1.96890351582499,1.,0.76122669048382));
#29396=CARTESIAN_POINT('Ctrl Pts',(-1.96264672744186,1.,0.761858300014423));
#29397=CARTESIAN_POINT('Ctrl Pts',(-1.95639665309869,1.,0.762447203806179));
#29398=CARTESIAN_POINT('Ctrl Pts',(-1.95015342590024,1.,0.762992990878769));
#29399=CARTESIAN_POINT('Ctrl Pts',(-1.9439174661764,1.,0.763495333538629));
#29400=CARTESIAN_POINT('Ctrl Pts',(-1.93768964875886,1.,0.763954049121458));
#29401=CARTESIAN_POINT('Ctrl Pts',(-1.93147105496382,1.,0.76436901067394));
#29402=CARTESIAN_POINT('Ctrl Pts',(-1.92526263537048,1.,0.764740025488211));
#29403=CARTESIAN_POINT('Ctrl Pts',(-1.91906491634196,1.,0.765066729667088));
#29404=CARTESIAN_POINT('Ctrl Pts',(-1.91287765805169,1.,0.765348465884722));
#29405=CARTESIAN_POINT('Ctrl Pts',(-1.90669961402356,1.,0.765584196937919));
#29406=CARTESIAN_POINT('Ctrl Pts',(-1.90052930393596,1.,0.765772772593386));
#29407=CARTESIAN_POINT('Ctrl Pts',(-1.89436577771388,1.,0.765913193856978));
#29408=CARTESIAN_POINT('Ctrl Pts',(-1.88820926433409,1.,0.766004837062091));
#29409=CARTESIAN_POINT('Ctrl Pts',(-1.88206215302561,1.,0.766047794851864));
#29410=CARTESIAN_POINT('Ctrl Pts',(-1.87592888967883,1.,0.766042837036744));
#29411=CARTESIAN_POINT('Ctrl Pts',(-1.86981398314341,1.,0.765990708546091));
#29412=CARTESIAN_POINT('Ctrl Pts',(-1.86372027063312,1.,0.765891519092547));
#29413=CARTESIAN_POINT('Ctrl Pts',(-1.85764741390394,1.,0.765744212909318));
#29414=CARTESIAN_POINT('Ctrl Pts',(-1.85158945130063,1.,0.765545710619062));
#29415=CARTESIAN_POINT('Ctrl Pts',(-1.84553698875924,1.,0.765291664862029));
#29416=CARTESIAN_POINT('Ctrl Pts',(-1.83948181064835,1.,0.764978057881737));
#29417=CARTESIAN_POINT('Ctrl Pts',(-1.83342077227142,1.,0.764602549687853));
#29418=CARTESIAN_POINT('Ctrl Pts',(-1.82735991200065,1.,0.764165902605995));
#29419=CARTESIAN_POINT('Ctrl Pts',(-1.82131873145266,1.,0.763673465462726));
#29420=CARTESIAN_POINT('Ctrl Pts',(-1.8153211840553,1.,0.763132003836634));
#29421=CARTESIAN_POINT('Ctrl Pts',(-1.80938551463965,1.,0.762546129463938));
#29422=CARTESIAN_POINT('Ctrl Pts',(-1.80351583877342,1.,0.761915336443547));
#29423=CARTESIAN_POINT('Ctrl Pts',(-1.79768986997783,1.,0.761229695230558));
#29424=CARTESIAN_POINT('Ctrl Pts',(-1.7918581561088,1.,0.760469555880749));
#29425=CARTESIAN_POINT('Ctrl Pts',(-1.78596964884604,1.,0.759614401110189));
#29426=CARTESIAN_POINT('Ctrl Pts',(-1.77999411220945,1.,0.758650626677518));
#29427=CARTESIAN_POINT('Ctrl Pts',(-1.77394167108292,1.,0.757578264077029));
#29428=CARTESIAN_POINT('Ctrl Pts',(-1.76789396002998,1.,0.75642189602781));
#29429=CARTESIAN_POINT('Ctrl Pts',(-1.76197817240128,1.,0.755220979974461));
#29430=CARTESIAN_POINT('Ctrl Pts',(-1.75631083600019,1.,0.754009254027829));
#29431=CARTESIAN_POINT('Ctrl Pts',(-1.75095139468794,1.,0.752797683531314));
#29432=CARTESIAN_POINT('Ctrl Pts',(-1.74585086852502,1.,0.751555614164482));
#29433=CARTESIAN_POINT('Ctrl Pts',(-1.74080458267114,1.,0.750193435981249));
#29434=CARTESIAN_POINT('Ctrl Pts',(-1.7355035168033,1.,0.74858246295687));
#29435=CARTESIAN_POINT('Ctrl Pts',(-1.72958533647714,1.,0.746574710097752));
#29436=CARTESIAN_POINT('Ctrl Pts',(-1.72268229916769,1.,0.744021445433093));
#29437=CARTESIAN_POINT('Ctrl Pts',(-1.71447789751001,1.,0.74079516202821));
#29438=CARTESIAN_POINT('Ctrl Pts',(-1.70473309004249,1.,0.736799665716932));
#29439=CARTESIAN_POINT('Ctrl Pts',(-1.69326921972915,1.,0.731963238685357));
#29440=CARTESIAN_POINT('Ctrl Pts',(-1.67996158451922,1.,0.726235967982445));
#29441=CARTESIAN_POINT('Ctrl Pts',(-1.66472880551777,1.,0.71958543378795));
#29442=CARTESIAN_POINT('Ctrl Pts',(-1.64752408828442,1.,0.711993139340447));
#29443=CARTESIAN_POINT('Ctrl Pts',(-1.6321654166204,1.,0.705159151977294));
#29444=CARTESIAN_POINT('Ctrl Pts',(-1.61974673471117,1.,0.699605146398837));
#29445=CARTESIAN_POINT('Ctrl Pts',(-1.61106790957619,1.,0.69571209787897));
#29446=CARTESIAN_POINT('Ctrl Pts',(-1.60662857109684,1.,0.693717979106305));
#29447=CARTESIAN_POINT('',(-2.0698113262342,0.,0.7455743247944));
#29448=CARTESIAN_POINT('Origin',(-2.11275013067528,0.,0.61342227326009));
#29449=CARTESIAN_POINT('',(-2.11275013067528,1.,0.61342227326009));
#29450=CARTESIAN_POINT('',(-2.0698113262342,1.,0.7455743247944));
#29451=CARTESIAN_POINT('',(-2.11275013067528,0.,0.61342227326009));
#29452=CARTESIAN_POINT('Ctrl Pts',(-1.7075470150345,-1.,0.383122945602004));
#29453=CARTESIAN_POINT('Ctrl Pts',(-1.7075470150345,1.,0.383122945602004));
#29454=CARTESIAN_POINT('Ctrl Pts',(-1.71231062891958,-1.,0.384119047315542));
#29455=CARTESIAN_POINT('Ctrl Pts',(-1.71231062891958,1.,0.384119047315542));
#29456=CARTESIAN_POINT('Ctrl Pts',(-1.72162022246158,-1.,0.38607079032701));
#29457=CARTESIAN_POINT('Ctrl Pts',(-1.72162022246158,1.,0.38607079032701));
#29458=CARTESIAN_POINT('Ctrl Pts',(-1.7349317097561,-1.,0.388877023509191));
#29459=CARTESIAN_POINT('Ctrl Pts',(-1.7349317097561,1.,0.388877023509191));
#29460=CARTESIAN_POINT('Ctrl Pts',(-1.75137405313962,-1.,0.392375812294307));
#29461=CARTESIAN_POINT('Ctrl Pts',(-1.75137405313962,1.,0.392375812294307));
#29462=CARTESIAN_POINT('Ctrl Pts',(-1.7697556004756,-1.,0.39634619612042));
#29463=CARTESIAN_POINT('Ctrl Pts',(-1.7697556004756,1.,0.39634619612042));
#29464=CARTESIAN_POINT('Ctrl Pts',(-1.78598826347533,-1.,0.39991940378308));
#29465=CARTESIAN_POINT('Ctrl Pts',(-1.78598826347533,1.,0.39991940378308));
#29466=CARTESIAN_POINT('Ctrl Pts',(-1.80012077176221,-1.,0.403107976170441));
#29467=CARTESIAN_POINT('Ctrl Pts',(-1.80012077176221,1.,0.403107976170441));
#29468=CARTESIAN_POINT('Ctrl Pts',(-1.81223801813988,-1.,0.405933518411838));
#29469=CARTESIAN_POINT('Ctrl Pts',(-1.81223801813988,1.,0.405933518411838));
#29470=CARTESIAN_POINT('Ctrl Pts',(-1.8224702267854,-1.,0.408428948108533));
#29471=CARTESIAN_POINT('Ctrl Pts',(-1.8224702267854,1.,0.408428948108533));
#29472=CARTESIAN_POINT('Ctrl Pts',(-1.83100408895216,-1.,0.410641256301675));
#29473=CARTESIAN_POINT('Ctrl Pts',(-1.83100408895216,1.,0.410641256301675));
#29474=CARTESIAN_POINT('Ctrl Pts',(-1.83808953475839,-1.,0.412633125322161));
#29475=CARTESIAN_POINT('Ctrl Pts',(-1.83808953475839,1.,0.412633125322161));
#29476=CARTESIAN_POINT('Ctrl Pts',(-1.8440575707371,-1.,0.41448743825434));
#29477=CARTESIAN_POINT('Ctrl Pts',(-1.8440575707371,1.,0.41448743825434));
#29478=CARTESIAN_POINT('Ctrl Pts',(-1.84929312929882,-1.,0.416300022038864));
#29479=CARTESIAN_POINT('Ctrl Pts',(-1.84929312929882,1.,0.416300022038864));
#29480=CARTESIAN_POINT('Ctrl Pts',(-1.85417632856234,-1.,0.418164129143534));
#29481=CARTESIAN_POINT('Ctrl Pts',(-1.85417632856234,1.,0.418164129143534));
#29482=CARTESIAN_POINT('Ctrl Pts',(-1.85903281096686,-1.,0.420157287975619));
#29483=CARTESIAN_POINT('Ctrl Pts',(-1.85903281096686,1.,0.420157287975619));
#29484=CARTESIAN_POINT('Ctrl Pts',(-1.86408083334028,-1.,0.422327307418275));
#29485=CARTESIAN_POINT('Ctrl Pts',(-1.86408083334028,1.,0.422327307418275));
#29486=CARTESIAN_POINT('Ctrl Pts',(-1.86937803944323,-1.,0.424678177291359));
#29487=CARTESIAN_POINT('Ctrl Pts',(-1.86937803944323,1.,0.424678177291359));
#29488=CARTESIAN_POINT('Ctrl Pts',(-1.87486989291484,-1.,0.427183828519102));
#29489=CARTESIAN_POINT('Ctrl Pts',(-1.87486989291484,1.,0.427183828519102));
#29490=CARTESIAN_POINT('Ctrl Pts',(-1.88044229001832,-1.,0.429803062482344));
#29491=CARTESIAN_POINT('Ctrl Pts',(-1.88044229001832,1.,0.429803062482344));
#29492=CARTESIAN_POINT('Ctrl Pts',(-1.88596913666793,-1.,0.432493038548748));
#29493=CARTESIAN_POINT('Ctrl Pts',(-1.88596913666793,1.,0.432493038548748));
#29494=CARTESIAN_POINT('Ctrl Pts',(-1.89136993975504,-1.,0.435225660963383));
#29495=CARTESIAN_POINT('Ctrl Pts',(-1.89136993975504,1.,0.435225660963383));
#29496=CARTESIAN_POINT('Ctrl Pts',(-1.89663648956466,-1.,0.437995003948244));
#29497=CARTESIAN_POINT('Ctrl Pts',(-1.89663648956466,1.,0.437995003948244));
#29498=CARTESIAN_POINT('Ctrl Pts',(-1.90180124389086,-1.,0.440807833704038));
#29499=CARTESIAN_POINT('Ctrl Pts',(-1.90180124389086,1.,0.440807833704038));
#29500=CARTESIAN_POINT('Ctrl Pts',(-1.90691756144898,-1.,0.44367755684915));
#29501=CARTESIAN_POINT('Ctrl Pts',(-1.90691756144898,1.,0.44367755684915));
#29502=CARTESIAN_POINT('Ctrl Pts',(-1.9120369998112,-1.,0.446617343485711));
#29503=CARTESIAN_POINT('Ctrl Pts',(-1.9120369998112,1.,0.446617343485711));
#29504=CARTESIAN_POINT('Ctrl Pts',(-1.91718342555755,-1.,0.449632260106662));
#29505=CARTESIAN_POINT('Ctrl Pts',(-1.91718342555755,1.,0.449632260106662));
#29506=CARTESIAN_POINT('Ctrl Pts',(-1.92235380648502,-1.,0.452719478359432));
#29507=CARTESIAN_POINT('Ctrl Pts',(-1.92235380648502,1.,0.452719478359432));
#29508=CARTESIAN_POINT('Ctrl Pts',(-1.92753067150476,-1.,0.455872005174371));
#29509=CARTESIAN_POINT('Ctrl Pts',(-1.92753067150476,1.,0.455872005174371));
#29510=CARTESIAN_POINT('Ctrl Pts',(-1.93269066517934,-1.,0.459081234547926));
#29511=CARTESIAN_POINT('Ctrl Pts',(-1.93269066517934,1.,0.459081234547926));
#29512=CARTESIAN_POINT('Ctrl Pts',(-1.93781486640821,-1.,0.462340031009056));
#29513=CARTESIAN_POINT('Ctrl Pts',(-1.93781486640821,1.,0.462340031009056));
#29514=CARTESIAN_POINT('Ctrl Pts',(-1.9428979419619,-1.,0.46564546202603));
#29515=CARTESIAN_POINT('Ctrl Pts',(-1.9428979419619,1.,0.46564546202603));
#29516=CARTESIAN_POINT('Ctrl Pts',(-1.94794381136514,-1.,0.468997482913135));
#29517=CARTESIAN_POINT('Ctrl Pts',(-1.94794381136514,1.,0.468997482913135));
#29518=CARTESIAN_POINT('Ctrl Pts',(-1.95296148278133,-1.,0.472397672264072));
#29519=CARTESIAN_POINT('Ctrl Pts',(-1.95296148278133,1.,0.472397672264072));
#29520=CARTESIAN_POINT('Ctrl Pts',(-1.95796111148177,-1.,0.475848034683176));
#29521=CARTESIAN_POINT('Ctrl Pts',(-1.95796111148177,1.,0.475848034683176));
#29522=CARTESIAN_POINT('Ctrl Pts',(-1.96294933055943,-1.,0.479349583074855));
#29523=CARTESIAN_POINT('Ctrl Pts',(-1.96294933055943,1.,0.479349583074855));
#29524=CARTESIAN_POINT('Ctrl Pts',(-1.96792703422362,-1.,0.48290166212069));
#29525=CARTESIAN_POINT('Ctrl Pts',(-1.96792703422362,1.,0.48290166212069));
#29526=CARTESIAN_POINT('Ctrl Pts',(-1.97289186263272,-1.,0.486502692907659));
#29527=CARTESIAN_POINT('Ctrl Pts',(-1.97289186263272,1.,0.486502692907659));
#29528=CARTESIAN_POINT('Ctrl Pts',(-1.97783973019229,-1.,0.490150627860952));
#29529=CARTESIAN_POINT('Ctrl Pts',(-1.97783973019229,1.,0.490150627860952));
#29530=CARTESIAN_POINT('Ctrl Pts',(-1.98276658761821,-1.,0.493843476541494));
#29531=CARTESIAN_POINT('Ctrl Pts',(-1.98276658761821,1.,0.493843476541494));
#29532=CARTESIAN_POINT('Ctrl Pts',(-1.98767044752932,-1.,0.497579909545574));
#29533=CARTESIAN_POINT('Ctrl Pts',(-1.98767044752932,1.,0.497579909545574));
#29534=CARTESIAN_POINT('Ctrl Pts',(-1.99255149126155,-1.,0.501359287727146));
#29535=CARTESIAN_POINT('Ctrl Pts',(-1.99255149126155,1.,0.501359287727146));
#29536=CARTESIAN_POINT('Ctrl Pts',(-1.99741107463572,-1.,0.505181361323026));
#29537=CARTESIAN_POINT('Ctrl Pts',(-1.99741107463572,1.,0.505181361323026));
#29538=CARTESIAN_POINT('Ctrl Pts',(-2.00225107134734,-1.,0.509046069886157));
#29539=CARTESIAN_POINT('Ctrl Pts',(-2.00225107134734,1.,0.509046069886157));
#29540=CARTESIAN_POINT('Ctrl Pts',(-2.00707309946949,-1.,0.512953306961792));
#29541=CARTESIAN_POINT('Ctrl Pts',(-2.00707309946949,1.,0.512953306961792));
#29542=CARTESIAN_POINT('Ctrl Pts',(-2.01187773939242,-1.,0.516902681728687));
#29543=CARTESIAN_POINT('Ctrl Pts',(-2.01187773939242,1.,0.516902681728687));
#29544=CARTESIAN_POINT('Ctrl Pts',(-2.01666477917286,-1.,0.52089359039937));
#29545=CARTESIAN_POINT('Ctrl Pts',(-2.01666477917286,1.,0.52089359039937));
#29546=CARTESIAN_POINT('Ctrl Pts',(-2.02143356304698,-1.,0.524925318333476));
#29547=CARTESIAN_POINT('Ctrl Pts',(-2.02143356304698,1.,0.524925318333476));
#29548=CARTESIAN_POINT('Ctrl Pts',(-2.0261832908329,-1.,0.528997127241914));
#29549=CARTESIAN_POINT('Ctrl Pts',(-2.0261832908329,1.,0.528997127241914));
#29550=CARTESIAN_POINT('Ctrl Pts',(-2.03091336214426,-1.,0.533108355132976));
#29551=CARTESIAN_POINT('Ctrl Pts',(-2.03091336214426,1.,0.533108355132976));
#29552=CARTESIAN_POINT('Ctrl Pts',(-2.03562362954037,-1.,0.537258489833262));
#29553=CARTESIAN_POINT('Ctrl Pts',(-2.03562362954037,1.,0.537258489833262));
#29554=CARTESIAN_POINT('Ctrl Pts',(-2.04031422690527,-1.,0.541447120615659));
#29555=CARTESIAN_POINT('Ctrl Pts',(-2.04031422690527,1.,0.541447120615659));
#29556=CARTESIAN_POINT('Ctrl Pts',(-2.04498544714588,-1.,0.54567390381743));
#29557=CARTESIAN_POINT('Ctrl Pts',(-2.04498544714588,1.,0.54567390381743));
#29558=CARTESIAN_POINT('Ctrl Pts',(-2.04963761077958,-1.,0.549938525150295));
#29559=CARTESIAN_POINT('Ctrl Pts',(-2.04963761077958,1.,0.549938525150295));
#29560=CARTESIAN_POINT('Ctrl Pts',(-2.05427091604413,-1.,0.554240657463906));
#29561=CARTESIAN_POINT('Ctrl Pts',(-2.05427091604413,1.,0.554240657463906));
#29562=CARTESIAN_POINT('Ctrl Pts',(-2.05888537756462,-1.,0.558579940185151));
#29563=CARTESIAN_POINT('Ctrl Pts',(-2.05888537756462,1.,0.558579940185151));
#29564=CARTESIAN_POINT('Ctrl Pts',(-2.06348090160589,-1.,0.562955993082261));
#29565=CARTESIAN_POINT('Ctrl Pts',(-2.06348090160589,1.,0.562955993082261));
#29566=CARTESIAN_POINT('Ctrl Pts',(-2.06805732997334,-1.,0.567368421181087));
#29567=CARTESIAN_POINT('Ctrl Pts',(-2.06805732997334,1.,0.567368421181087));
#29568=CARTESIAN_POINT('Ctrl Pts',(-2.07261449292824,-1.,0.571816823242603));
#29569=CARTESIAN_POINT('Ctrl Pts',(-2.07261449292824,1.,0.571816823242603));
#29570=CARTESIAN_POINT('Ctrl Pts',(-2.07715226767559,-1.,0.576300797416844));
#29571=CARTESIAN_POINT('Ctrl Pts',(-2.07715226767559,1.,0.576300797416844));
#29572=CARTESIAN_POINT('Ctrl Pts',(-2.08167059018418,-1.,0.580819952108063));
#29573=CARTESIAN_POINT('Ctrl Pts',(-2.08167059018418,1.,0.580819952108063));
#29574=CARTESIAN_POINT('Ctrl Pts',(-2.08616943727951,-1.,0.585373918991617));
#29575=CARTESIAN_POINT('Ctrl Pts',(-2.08616943727951,1.,0.585373918991617));
#29576=CARTESIAN_POINT('Ctrl Pts',(-2.09064881812129,-1.,0.589962365403406));
#29577=CARTESIAN_POINT('Ctrl Pts',(-2.09064881812129,1.,0.589962365403406));
#29578=CARTESIAN_POINT('Ctrl Pts',(-2.0951087622027,-1.,0.594585006052162));
#29579=CARTESIAN_POINT('Ctrl Pts',(-2.0951087622027,1.,0.594585006052162));
#29580=CARTESIAN_POINT('Ctrl Pts',(-2.0995493086477,-1.,0.599241616420533));
#29581=CARTESIAN_POINT('Ctrl Pts',(-2.0995493086477,1.,0.599241616420533));
#29582=CARTESIAN_POINT('Ctrl Pts',(-2.10397049886949,-1.,0.60393203073603));
#29583=CARTESIAN_POINT('Ctrl Pts',(-2.10397049886949,1.,0.60393203073603));
#29584=CARTESIAN_POINT('Ctrl Pts',(-2.1074919961518,-1.,0.607711315454876));
#29585=CARTESIAN_POINT('Ctrl Pts',(-2.1074919961518,1.,0.607711315454876));
#29586=CARTESIAN_POINT('Ctrl Pts',(-2.11012443807238,-1.,0.610560911689899));
#29587=CARTESIAN_POINT('Ctrl Pts',(-2.11012443807238,1.,0.610560911689899));
#29588=CARTESIAN_POINT('Ctrl Pts',(-2.11187554259986,-1.,0.6124673655618));
#29589=CARTESIAN_POINT('Ctrl Pts',(-2.11187554259986,1.,0.6124673655618));
#29590=CARTESIAN_POINT('Ctrl Pts',(-2.11275013067528,-1.,0.61342227326009));
#29591=CARTESIAN_POINT('Ctrl Pts',(-2.11275013067528,1.,0.61342227326009));
#29592=CARTESIAN_POINT('',(-1.7075470150345,1.,0.383122945602004));
#29593=CARTESIAN_POINT('Ctrl Pts',(-1.7075470150345,1.,0.383122945602004));
#29594=CARTESIAN_POINT('Ctrl Pts',(-1.71231062891958,1.,0.384119047315542));
#29595=CARTESIAN_POINT('Ctrl Pts',(-1.72162022246158,1.,0.38607079032701));
#29596=CARTESIAN_POINT('Ctrl Pts',(-1.7349317097561,1.,0.388877023509191));
#29597=CARTESIAN_POINT('Ctrl Pts',(-1.75137405313962,1.,0.392375812294307));
#29598=CARTESIAN_POINT('Ctrl Pts',(-1.7697556004756,1.,0.39634619612042));
#29599=CARTESIAN_POINT('Ctrl Pts',(-1.78598826347533,1.,0.39991940378308));
#29600=CARTESIAN_POINT('Ctrl Pts',(-1.80012077176221,1.,0.403107976170441));
#29601=CARTESIAN_POINT('Ctrl Pts',(-1.81223801813988,1.,0.405933518411838));
#29602=CARTESIAN_POINT('Ctrl Pts',(-1.8224702267854,1.,0.408428948108533));
#29603=CARTESIAN_POINT('Ctrl Pts',(-1.83100408895216,1.,0.410641256301675));
#29604=CARTESIAN_POINT('Ctrl Pts',(-1.83808953475839,1.,0.412633125322161));
#29605=CARTESIAN_POINT('Ctrl Pts',(-1.8440575707371,1.,0.41448743825434));
#29606=CARTESIAN_POINT('Ctrl Pts',(-1.84929312929882,1.,0.416300022038864));
#29607=CARTESIAN_POINT('Ctrl Pts',(-1.85417632856234,1.,0.418164129143534));
#29608=CARTESIAN_POINT('Ctrl Pts',(-1.85903281096686,1.,0.420157287975619));
#29609=CARTESIAN_POINT('Ctrl Pts',(-1.86408083334028,1.,0.422327307418275));
#29610=CARTESIAN_POINT('Ctrl Pts',(-1.86937803944323,1.,0.424678177291359));
#29611=CARTESIAN_POINT('Ctrl Pts',(-1.87486989291484,1.,0.427183828519102));
#29612=CARTESIAN_POINT('Ctrl Pts',(-1.88044229001832,1.,0.429803062482344));
#29613=CARTESIAN_POINT('Ctrl Pts',(-1.88596913666793,1.,0.432493038548748));
#29614=CARTESIAN_POINT('Ctrl Pts',(-1.89136993975504,1.,0.435225660963383));
#29615=CARTESIAN_POINT('Ctrl Pts',(-1.89663648956466,1.,0.437995003948244));
#29616=CARTESIAN_POINT('Ctrl Pts',(-1.90180124389086,1.,0.440807833704038));
#29617=CARTESIAN_POINT('Ctrl Pts',(-1.90691756144898,1.,0.44367755684915));
#29618=CARTESIAN_POINT('Ctrl Pts',(-1.9120369998112,1.,0.446617343485711));
#29619=CARTESIAN_POINT('Ctrl Pts',(-1.91718342555755,1.,0.449632260106662));
#29620=CARTESIAN_POINT('Ctrl Pts',(-1.92235380648502,1.,0.452719478359432));
#29621=CARTESIAN_POINT('Ctrl Pts',(-1.92753067150476,1.,0.455872005174371));
#29622=CARTESIAN_POINT('Ctrl Pts',(-1.93269066517934,1.,0.459081234547926));
#29623=CARTESIAN_POINT('Ctrl Pts',(-1.93781486640821,1.,0.462340031009056));
#29624=CARTESIAN_POINT('Ctrl Pts',(-1.9428979419619,1.,0.46564546202603));
#29625=CARTESIAN_POINT('Ctrl Pts',(-1.94794381136514,1.,0.468997482913135));
#29626=CARTESIAN_POINT('Ctrl Pts',(-1.95296148278133,1.,0.472397672264072));
#29627=CARTESIAN_POINT('Ctrl Pts',(-1.95796111148177,1.,0.475848034683176));
#29628=CARTESIAN_POINT('Ctrl Pts',(-1.96294933055943,1.,0.479349583074855));
#29629=CARTESIAN_POINT('Ctrl Pts',(-1.96792703422362,1.,0.48290166212069));
#29630=CARTESIAN_POINT('Ctrl Pts',(-1.97289186263272,1.,0.486502692907659));
#29631=CARTESIAN_POINT('Ctrl Pts',(-1.97783973019229,1.,0.490150627860952));
#29632=CARTESIAN_POINT('Ctrl Pts',(-1.98276658761821,1.,0.493843476541494));
#29633=CARTESIAN_POINT('Ctrl Pts',(-1.98767044752932,1.,0.497579909545574));
#29634=CARTESIAN_POINT('Ctrl Pts',(-1.99255149126155,1.,0.501359287727146));
#29635=CARTESIAN_POINT('Ctrl Pts',(-1.99741107463572,1.,0.505181361323026));
#29636=CARTESIAN_POINT('Ctrl Pts',(-2.00225107134734,1.,0.509046069886157));
#29637=CARTESIAN_POINT('Ctrl Pts',(-2.00707309946949,1.,0.512953306961792));
#29638=CARTESIAN_POINT('Ctrl Pts',(-2.01187773939242,1.,0.516902681728687));
#29639=CARTESIAN_POINT('Ctrl Pts',(-2.01666477917286,1.,0.52089359039937));
#29640=CARTESIAN_POINT('Ctrl Pts',(-2.02143356304698,1.,0.524925318333476));
#29641=CARTESIAN_POINT('Ctrl Pts',(-2.0261832908329,1.,0.528997127241914));
#29642=CARTESIAN_POINT('Ctrl Pts',(-2.03091336214426,1.,0.533108355132976));
#29643=CARTESIAN_POINT('Ctrl Pts',(-2.03562362954037,1.,0.537258489833262));
#29644=CARTESIAN_POINT('Ctrl Pts',(-2.04031422690527,1.,0.541447120615659));
#29645=CARTESIAN_POINT('Ctrl Pts',(-2.04498544714588,1.,0.54567390381743));
#29646=CARTESIAN_POINT('Ctrl Pts',(-2.04963761077958,1.,0.549938525150295));
#29647=CARTESIAN_POINT('Ctrl Pts',(-2.05427091604413,1.,0.554240657463906));
#29648=CARTESIAN_POINT('Ctrl Pts',(-2.05888537756462,1.,0.558579940185151));
#29649=CARTESIAN_POINT('Ctrl Pts',(-2.06348090160589,1.,0.562955993082261));
#29650=CARTESIAN_POINT('Ctrl Pts',(-2.06805732997334,1.,0.567368421181087));
#29651=CARTESIAN_POINT('Ctrl Pts',(-2.07261449292824,1.,0.571816823242603));
#29652=CARTESIAN_POINT('Ctrl Pts',(-2.07715226767559,1.,0.576300797416844));
#29653=CARTESIAN_POINT('Ctrl Pts',(-2.08167059018418,1.,0.580819952108063));
#29654=CARTESIAN_POINT('Ctrl Pts',(-2.08616943727951,1.,0.585373918991617));
#29655=CARTESIAN_POINT('Ctrl Pts',(-2.09064881812129,1.,0.589962365403406));
#29656=CARTESIAN_POINT('Ctrl Pts',(-2.0951087622027,1.,0.594585006052162));
#29657=CARTESIAN_POINT('Ctrl Pts',(-2.0995493086477,1.,0.599241616420533));
#29658=CARTESIAN_POINT('Ctrl Pts',(-2.10397049886949,1.,0.60393203073603));
#29659=CARTESIAN_POINT('Ctrl Pts',(-2.1074919961518,1.,0.607711315454876));
#29660=CARTESIAN_POINT('Ctrl Pts',(-2.11012443807238,1.,0.610560911689899));
#29661=CARTESIAN_POINT('Ctrl Pts',(-2.11187554259986,1.,0.6124673655618));
#29662=CARTESIAN_POINT('Ctrl Pts',(-2.11275013067528,1.,0.61342227326009));
#29663=CARTESIAN_POINT('',(-1.7075470150345,0.,0.383122945602003));
#29664=CARTESIAN_POINT('Origin',(0.,0.,0.));
#29665=CARTESIAN_POINT('',(-1.74236521665491,1.,0.163289472382896));
#29666=CARTESIAN_POINT('Origin',(0.,1.,0.));
#29667=CARTESIAN_POINT('',(-1.74236521665491,0.,0.163289472382896));
#29668=CARTESIAN_POINT('Ctrl Pts',(-2.19890268624765,-1.,0.069476445021958));
#29669=CARTESIAN_POINT('Ctrl Pts',(-2.19890268624765,1.,0.069476445021958));
#29670=CARTESIAN_POINT('Ctrl Pts',(-2.19777582085423,-1.,0.0701143536325489));
#29671=CARTESIAN_POINT('Ctrl Pts',(-2.19777582085423,1.,0.0701143536325489));
#29672=CARTESIAN_POINT('Ctrl Pts',(-2.19552129484002,-1.,0.0713863779526153));
#29673=CARTESIAN_POINT('Ctrl Pts',(-2.19552129484002,1.,0.0713863779526153));
#29674=CARTESIAN_POINT('Ctrl Pts',(-2.19213712013662,-1.,0.0732830357306724));
#29675=CARTESIAN_POINT('Ctrl Pts',(-2.19213712013662,1.,0.0732830357306724));
#29676=CARTESIAN_POINT('Ctrl Pts',(-2.1876201139953,-1.,0.0757891465836146));
#29677=CARTESIAN_POINT('Ctrl Pts',(-2.1876201139953,1.,0.0757891465836146));
#29678=CARTESIAN_POINT('Ctrl Pts',(-2.18196589448887,-1.,0.0788837727685241));
#29679=CARTESIAN_POINT('Ctrl Pts',(-2.18196589448887,1.,0.0788837727685241));
#29680=CARTESIAN_POINT('Ctrl Pts',(-2.176303712113,-1.,0.0819402680872764));
#29681=CARTESIAN_POINT('Ctrl Pts',(-2.176303712113,1.,0.0819402680872764));
#29682=CARTESIAN_POINT('Ctrl Pts',(-2.17063357870952,-1.,0.0849584620835371));
#29683=CARTESIAN_POINT('Ctrl Pts',(-2.17063357870952,1.,0.0849584620835371));
#29684=CARTESIAN_POINT('Ctrl Pts',(-2.16495552645014,-1.,0.0879381291386921));
#29685=CARTESIAN_POINT('Ctrl Pts',(-2.16495552645014,1.,0.0879381291386921));
#29686=CARTESIAN_POINT('Ctrl Pts',(-2.15926961544516,-1.,0.0908789888107264));
#29687=CARTESIAN_POINT('Ctrl Pts',(-2.15926961544516,1.,0.0908789888107264));
#29688=CARTESIAN_POINT('Ctrl Pts',(-2.1535759397817,-1.,0.0937807218867642));
#29689=CARTESIAN_POINT('Ctrl Pts',(-2.1535759397817,1.,0.0937807218867642));
#29690=CARTESIAN_POINT('Ctrl Pts',(-2.14787463531795,-1.,0.0966429852305457));
#29691=CARTESIAN_POINT('Ctrl Pts',(-2.14787463531795,1.,0.0966429852305457));
#29692=CARTESIAN_POINT('Ctrl Pts',(-2.14216588396025,-1.,0.0994654261990914));
#29693=CARTESIAN_POINT('Ctrl Pts',(-2.14216588396025,1.,0.0994654261990914));
#29694=CARTESIAN_POINT('Ctrl Pts',(-2.13644992667165,-1.,0.1022477005561));
#29695=CARTESIAN_POINT('Ctrl Pts',(-2.13644992667165,1.,0.1022477005561));
#29696=CARTESIAN_POINT('Ctrl Pts',(-2.13072704887293,-1.,0.104989479152739));
#29697=CARTESIAN_POINT('Ctrl Pts',(-2.13072704887293,1.,0.104989479152739));
#29698=CARTESIAN_POINT('Ctrl Pts',(-2.12499752307,-1.,0.10769043523109));
#29699=CARTESIAN_POINT('Ctrl Pts',(-2.12499752307,1.,0.10769043523109));
#29700=CARTESIAN_POINT('Ctrl Pts',(-2.11926155590865,-1.,0.110350236135025));
#29701=CARTESIAN_POINT('Ctrl Pts',(-2.11926155590865,1.,0.110350236135025));
#29702=CARTESIAN_POINT('Ctrl Pts',(-2.11351924490306,-1.,0.112968534419737));
#29703=CARTESIAN_POINT('Ctrl Pts',(-2.11351924490306,1.,0.112968534419737));
#29704=CARTESIAN_POINT('Ctrl Pts',(-2.10777050261309,-1.,0.115544957687926));
#29705=CARTESIAN_POINT('Ctrl Pts',(-2.10777050261309,1.,0.115544957687926));
#29706=CARTESIAN_POINT('Ctrl Pts',(-2.102015121329,-1.,0.118079107988355));
#29707=CARTESIAN_POINT('Ctrl Pts',(-2.102015121329,1.,0.118079107988355));
#29708=CARTESIAN_POINT('Ctrl Pts',(-2.0962529286773,-1.,0.120570567965122));
#29709=CARTESIAN_POINT('Ctrl Pts',(-2.0962529286773,1.,0.120570567965122));
#29710=CARTESIAN_POINT('Ctrl Pts',(-2.09048392424825,-1.,0.123018905621083));
#29711=CARTESIAN_POINT('Ctrl Pts',(-2.09048392424825,1.,0.123018905621083));
#29712=CARTESIAN_POINT('Ctrl Pts',(-2.08470840653643,-1.,0.125423679412061));
#29713=CARTESIAN_POINT('Ctrl Pts',(-2.08470840653643,1.,0.125423679412061));
#29714=CARTESIAN_POINT('Ctrl Pts',(-2.07892715110987,-1.,0.12778444527612));
#29715=CARTESIAN_POINT('Ctrl Pts',(-2.07892715110987,1.,0.12778444527612));
#29716=CARTESIAN_POINT('Ctrl Pts',(-2.07314114713063,-1.,0.130100748328403));
#29717=CARTESIAN_POINT('Ctrl Pts',(-2.07314114713063,1.,0.130100748328403));
#29718=CARTESIAN_POINT('Ctrl Pts',(-2.06735123910326,-1.,0.13237211154771));
#29719=CARTESIAN_POINT('Ctrl Pts',(-2.06735123910326,1.,0.13237211154771));
#29720=CARTESIAN_POINT('Ctrl Pts',(-2.06155781517842,-1.,0.134598026192106));
#29721=CARTESIAN_POINT('Ctrl Pts',(-2.06155781517842,1.,0.134598026192106));
#29722=CARTESIAN_POINT('Ctrl Pts',(-2.05576044414264,-1.,0.136777941218043));
#29723=CARTESIAN_POINT('Ctrl Pts',(-2.05576044414264,1.,0.136777941218043));
#29724=CARTESIAN_POINT('Ctrl Pts',(-2.04995762001328,-1.,0.138911255368966));
#29725=CARTESIAN_POINT('Ctrl Pts',(-2.04995762001328,1.,0.138911255368966));
#29726=CARTESIAN_POINT('Ctrl Pts',(-2.04414757947916,-1.,0.140997332152546));
#29727=CARTESIAN_POINT('Ctrl Pts',(-2.04414757947916,1.,0.140997332152546));
#29728=CARTESIAN_POINT('Ctrl Pts',(-2.03832911025912,-1.,0.143035515058209));
#29729=CARTESIAN_POINT('Ctrl Pts',(-2.03832911025912,1.,0.143035515058209));
#29730=CARTESIAN_POINT('Ctrl Pts',(-2.03250223739942,-1.,0.145025140186057));
#29731=CARTESIAN_POINT('Ctrl Pts',(-2.03250223739942,1.,0.145025140186057));
#29732=CARTESIAN_POINT('Ctrl Pts',(-2.02666926182017,-1.,0.146965557332583));
#29733=CARTESIAN_POINT('Ctrl Pts',(-2.02666926182017,1.,0.146965557332583));
#29734=CARTESIAN_POINT('Ctrl Pts',(-2.02083464969894,-1.,0.148856124775337));
#29735=CARTESIAN_POINT('Ctrl Pts',(-2.02083464969894,1.,0.148856124775337));
#29736=CARTESIAN_POINT('Ctrl Pts',(-2.01500291940238,-1.,0.150696157673078));
#29737=CARTESIAN_POINT('Ctrl Pts',(-2.01500291940238,1.,0.150696157673078));
#29738=CARTESIAN_POINT('Ctrl Pts',(-2.00917680318424,-1.,0.15248488362145));
#29739=CARTESIAN_POINT('Ctrl Pts',(-2.00917680318424,1.,0.15248488362145));
#29740=CARTESIAN_POINT('Ctrl Pts',(-2.00335565310543,-1.,0.154221403049722));
#29741=CARTESIAN_POINT('Ctrl Pts',(-2.00335565310543,1.,0.154221403049722));
#29742=CARTESIAN_POINT('Ctrl Pts',(-1.99753284771497,-1.,0.155904629548783));
#29743=CARTESIAN_POINT('Ctrl Pts',(-1.99753284771497,1.,0.155904629548783));
#29744=CARTESIAN_POINT('Ctrl Pts',(-1.99169810931908,-1.,0.157533331459227));
#29745=CARTESIAN_POINT('Ctrl Pts',(-1.99169810931908,1.,0.157533331459227));
#29746=CARTESIAN_POINT('Ctrl Pts',(-1.98584238283292,-1.,0.159106226437299));
#29747=CARTESIAN_POINT('Ctrl Pts',(-1.98584238283292,1.,0.159106226437299));
#29748=CARTESIAN_POINT('Ctrl Pts',(-1.97996195437559,-1.,0.160622060784611));
#29749=CARTESIAN_POINT('Ctrl Pts',(-1.97996195437559,1.,0.160622060784611));
#29750=CARTESIAN_POINT('Ctrl Pts',(-1.97406280235188,-1.,0.162079693556288));
#29751=CARTESIAN_POINT('Ctrl Pts',(-1.97406280235188,1.,0.162079693556288));
#29752=CARTESIAN_POINT('Ctrl Pts',(-1.96816512677967,-1.,0.163478185457734));
#29753=CARTESIAN_POINT('Ctrl Pts',(-1.96816512677967,1.,0.163478185457734));
#29754=CARTESIAN_POINT('Ctrl Pts',(-1.96229379940136,-1.,0.164816568920269));
#29755=CARTESIAN_POINT('Ctrl Pts',(-1.96229379940136,1.,0.164816568920269));
#29756=CARTESIAN_POINT('Ctrl Pts',(-1.9564675971873,-1.,0.166093592002812));
#29757=CARTESIAN_POINT('Ctrl Pts',(-1.9564675971873,1.,0.166093592002812));
#29758=CARTESIAN_POINT('Ctrl Pts',(-1.95069027794294,-1.,0.167307501784475));
#29759=CARTESIAN_POINT('Ctrl Pts',(-1.95069027794294,1.,0.167307501784475));
#29760=CARTESIAN_POINT('Ctrl Pts',(-1.94493757756931,-1.,0.168455741607556));
#29761=CARTESIAN_POINT('Ctrl Pts',(-1.94493757756931,1.,0.168455741607556));
#29762=CARTESIAN_POINT('Ctrl Pts',(-1.93915639211581,-1.,0.169534904817491));
#29763=CARTESIAN_POINT('Ctrl Pts',(-1.93915639211581,1.,0.169534904817491));
#29764=CARTESIAN_POINT('Ctrl Pts',(-1.93329183155539,-1.,0.170541253116201));
#29765=CARTESIAN_POINT('Ctrl Pts',(-1.93329183155539,1.,0.170541253116201));
#29766=CARTESIAN_POINT('Ctrl Pts',(-1.92731093582036,-1.,0.171471191532988));
#29767=CARTESIAN_POINT('Ctrl Pts',(-1.92731093582036,1.,0.171471191532988));
#29768=CARTESIAN_POINT('Ctrl Pts',(-1.9212233439798,-1.,0.172321621259514));
#29769=CARTESIAN_POINT('Ctrl Pts',(-1.9212233439798,1.,0.172321621259514));
#29770=CARTESIAN_POINT('Ctrl Pts',(-1.91511429159527,-1.,0.173090695383496));
#29771=CARTESIAN_POINT('Ctrl Pts',(-1.91511429159527,1.,0.173090695383496));
#29772=CARTESIAN_POINT('Ctrl Pts',(-1.90911693975267,-1.,0.173776635257817));
#29773=CARTESIAN_POINT('Ctrl Pts',(-1.90911693975267,1.,0.173776635257817));
#29774=CARTESIAN_POINT('Ctrl Pts',(-1.90335253862834,-1.,0.174375518661085));
#29775=CARTESIAN_POINT('Ctrl Pts',(-1.90335253862834,1.,0.174375518661085));
#29776=CARTESIAN_POINT('Ctrl Pts',(-1.89788101117132,-1.,0.174879405091263));
#29777=CARTESIAN_POINT('Ctrl Pts',(-1.89788101117132,1.,0.174879405091263));
#29778=CARTESIAN_POINT('Ctrl Pts',(-1.892646301985,-1.,0.175274276190844));
#29779=CARTESIAN_POINT('Ctrl Pts',(-1.892646301985,1.,0.175274276190844));
#29780=CARTESIAN_POINT('Ctrl Pts',(-1.88742606273259,-1.,0.175538155840648));
#29781=CARTESIAN_POINT('Ctrl Pts',(-1.88742606273259,1.,0.175538155840648));
#29782=CARTESIAN_POINT('Ctrl Pts',(-1.88188663145367,-1.,0.175644148889698));
#29783=CARTESIAN_POINT('Ctrl Pts',(-1.88188663145367,1.,0.175644148889698));
#29784=CARTESIAN_POINT('Ctrl Pts',(-1.87563767773588,-1.,0.175563480746485));
#29785=CARTESIAN_POINT('Ctrl Pts',(-1.87563767773588,1.,0.175563480746485));
#29786=CARTESIAN_POINT('Ctrl Pts',(-1.86828349694799,-1.,0.175268337590758));
#29787=CARTESIAN_POINT('Ctrl Pts',(-1.86828349694799,1.,0.175268337590758));
#29788=CARTESIAN_POINT('Ctrl Pts',(-1.85948367088837,-1.,0.17473525927603));
#29789=CARTESIAN_POINT('Ctrl Pts',(-1.85948367088837,1.,0.17473525927603));
#29790=CARTESIAN_POINT('Ctrl Pts',(-1.8489811319852,-1.,0.173946627587731));
#29791=CARTESIAN_POINT('Ctrl Pts',(-1.8489811319852,1.,0.173946627587731));
#29792=CARTESIAN_POINT('Ctrl Pts',(-1.83658380527692,-1.,0.1728894428919));
#29793=CARTESIAN_POINT('Ctrl Pts',(-1.83658380527692,1.,0.1728894428919));
#29794=CARTESIAN_POINT('Ctrl Pts',(-1.82215766811545,-1.,0.171554770204119));
#29795=CARTESIAN_POINT('Ctrl Pts',(-1.82215766811545,1.,0.171554770204119));
#29796=CARTESIAN_POINT('Ctrl Pts',(-1.80561530629706,-1.,0.169936923904608));
#29797=CARTESIAN_POINT('Ctrl Pts',(-1.80561530629706,1.,0.169936923904608));
#29798=CARTESIAN_POINT('Ctrl Pts',(-1.7869064998507,-1.,0.168032772805197));
#29799=CARTESIAN_POINT('Ctrl Pts',(-1.7869064998507,1.,0.168032772805197));
#29800=CARTESIAN_POINT('Ctrl Pts',(-1.77018771684844,-1.,0.1662793551464));
#29801=CARTESIAN_POINT('Ctrl Pts',(-1.77018771684844,1.,0.1662793551464));
#29802=CARTESIAN_POINT('Ctrl Pts',(-1.75666056638427,-1.,0.164834765707158));
#29803=CARTESIAN_POINT('Ctrl Pts',(-1.75666056638427,1.,0.164834765707158));
#29804=CARTESIAN_POINT('Ctrl Pts',(-1.7472034950333,-1.,0.163814161002002));
#29805=CARTESIAN_POINT('Ctrl Pts',(-1.7472034950333,1.,0.163814161002002));
#29806=CARTESIAN_POINT('Ctrl Pts',(-1.74236521665491,-1.,0.163289472382896));
#29807=CARTESIAN_POINT('Ctrl Pts',(-1.74236521665491,1.,0.163289472382896));
#29808=CARTESIAN_POINT('',(-2.19890268624765,1.,0.069476445021958));
#29809=CARTESIAN_POINT('Ctrl Pts',(-2.19890268624765,1.,0.069476445021958));
#29810=CARTESIAN_POINT('Ctrl Pts',(-2.19777582085423,1.,0.0701143536325489));
#29811=CARTESIAN_POINT('Ctrl Pts',(-2.19552129484002,1.,0.0713863779526153));
#29812=CARTESIAN_POINT('Ctrl Pts',(-2.19213712013662,1.,0.0732830357306724));
#29813=CARTESIAN_POINT('Ctrl Pts',(-2.1876201139953,1.,0.0757891465836146));
#29814=CARTESIAN_POINT('Ctrl Pts',(-2.18196589448887,1.,0.0788837727685241));
#29815=CARTESIAN_POINT('Ctrl Pts',(-2.176303712113,1.,0.0819402680872764));
#29816=CARTESIAN_POINT('Ctrl Pts',(-2.17063357870952,1.,0.0849584620835371));
#29817=CARTESIAN_POINT('Ctrl Pts',(-2.16495552645014,1.,0.0879381291386921));
#29818=CARTESIAN_POINT('Ctrl Pts',(-2.15926961544516,1.,0.0908789888107264));
#29819=CARTESIAN_POINT('Ctrl Pts',(-2.1535759397817,1.,0.0937807218867642));
#29820=CARTESIAN_POINT('Ctrl Pts',(-2.14787463531795,1.,0.0966429852305457));
#29821=CARTESIAN_POINT('Ctrl Pts',(-2.14216588396025,1.,0.0994654261990914));
#29822=CARTESIAN_POINT('Ctrl Pts',(-2.13644992667165,1.,0.1022477005561));
#29823=CARTESIAN_POINT('Ctrl Pts',(-2.13072704887293,1.,0.104989479152739));
#29824=CARTESIAN_POINT('Ctrl Pts',(-2.12499752307,1.,0.10769043523109));
#29825=CARTESIAN_POINT('Ctrl Pts',(-2.11926155590865,1.,0.110350236135025));
#29826=CARTESIAN_POINT('Ctrl Pts',(-2.11351924490306,1.,0.112968534419737));
#29827=CARTESIAN_POINT('Ctrl Pts',(-2.10777050261309,1.,0.115544957687926));
#29828=CARTESIAN_POINT('Ctrl Pts',(-2.102015121329,1.,0.118079107988355));
#29829=CARTESIAN_POINT('Ctrl Pts',(-2.0962529286773,1.,0.120570567965122));
#29830=CARTESIAN_POINT('Ctrl Pts',(-2.09048392424825,1.,0.123018905621083));
#29831=CARTESIAN_POINT('Ctrl Pts',(-2.08470840653643,1.,0.125423679412061));
#29832=CARTESIAN_POINT('Ctrl Pts',(-2.07892715110987,1.,0.12778444527612));
#29833=CARTESIAN_POINT('Ctrl Pts',(-2.07314114713063,1.,0.130100748328403));
#29834=CARTESIAN_POINT('Ctrl Pts',(-2.06735123910326,1.,0.13237211154771));
#29835=CARTESIAN_POINT('Ctrl Pts',(-2.06155781517842,1.,0.134598026192106));
#29836=CARTESIAN_POINT('Ctrl Pts',(-2.05576044414264,1.,0.136777941218043));
#29837=CARTESIAN_POINT('Ctrl Pts',(-2.04995762001328,1.,0.138911255368966));
#29838=CARTESIAN_POINT('Ctrl Pts',(-2.04414757947916,1.,0.140997332152546));
#29839=CARTESIAN_POINT('Ctrl Pts',(-2.03832911025912,1.,0.143035515058209));
#29840=CARTESIAN_POINT('Ctrl Pts',(-2.03250223739942,1.,0.145025140186057));
#29841=CARTESIAN_POINT('Ctrl Pts',(-2.02666926182017,1.,0.146965557332583));
#29842=CARTESIAN_POINT('Ctrl Pts',(-2.02083464969894,1.,0.148856124775337));
#29843=CARTESIAN_POINT('Ctrl Pts',(-2.01500291940238,1.,0.150696157673078));
#29844=CARTESIAN_POINT('Ctrl Pts',(-2.00917680318424,1.,0.15248488362145));
#29845=CARTESIAN_POINT('Ctrl Pts',(-2.00335565310543,1.,0.154221403049722));
#29846=CARTESIAN_POINT('Ctrl Pts',(-1.99753284771497,1.,0.155904629548783));
#29847=CARTESIAN_POINT('Ctrl Pts',(-1.99169810931908,1.,0.157533331459227));
#29848=CARTESIAN_POINT('Ctrl Pts',(-1.98584238283292,1.,0.159106226437299));
#29849=CARTESIAN_POINT('Ctrl Pts',(-1.97996195437559,1.,0.160622060784611));
#29850=CARTESIAN_POINT('Ctrl Pts',(-1.97406280235188,1.,0.162079693556288));
#29851=CARTESIAN_POINT('Ctrl Pts',(-1.96816512677967,1.,0.163478185457734));
#29852=CARTESIAN_POINT('Ctrl Pts',(-1.96229379940136,1.,0.164816568920269));
#29853=CARTESIAN_POINT('Ctrl Pts',(-1.9564675971873,1.,0.166093592002812));
#29854=CARTESIAN_POINT('Ctrl Pts',(-1.95069027794294,1.,0.167307501784475));
#29855=CARTESIAN_POINT('Ctrl Pts',(-1.94493757756931,1.,0.168455741607556));
#29856=CARTESIAN_POINT('Ctrl Pts',(-1.93915639211581,1.,0.169534904817491));
#29857=CARTESIAN_POINT('Ctrl Pts',(-1.93329183155539,1.,0.170541253116201));
#29858=CARTESIAN_POINT('Ctrl Pts',(-1.92731093582036,1.,0.171471191532988));
#29859=CARTESIAN_POINT('Ctrl Pts',(-1.9212233439798,1.,0.172321621259514));
#29860=CARTESIAN_POINT('Ctrl Pts',(-1.91511429159527,1.,0.173090695383496));
#29861=CARTESIAN_POINT('Ctrl Pts',(-1.90911693975267,1.,0.173776635257817));
#29862=CARTESIAN_POINT('Ctrl Pts',(-1.90335253862834,1.,0.174375518661085));
#29863=CARTESIAN_POINT('Ctrl Pts',(-1.89788101117132,1.,0.174879405091263));
#29864=CARTESIAN_POINT('Ctrl Pts',(-1.892646301985,1.,0.175274276190844));
#29865=CARTESIAN_POINT('Ctrl Pts',(-1.88742606273259,1.,0.175538155840648));
#29866=CARTESIAN_POINT('Ctrl Pts',(-1.88188663145367,1.,0.175644148889698));
#29867=CARTESIAN_POINT('Ctrl Pts',(-1.87563767773588,1.,0.175563480746485));
#29868=CARTESIAN_POINT('Ctrl Pts',(-1.86828349694799,1.,0.175268337590758));
#29869=CARTESIAN_POINT('Ctrl Pts',(-1.85948367088837,1.,0.17473525927603));
#29870=CARTESIAN_POINT('Ctrl Pts',(-1.8489811319852,1.,0.173946627587731));
#29871=CARTESIAN_POINT('Ctrl Pts',(-1.83658380527692,1.,0.1728894428919));
#29872=CARTESIAN_POINT('Ctrl Pts',(-1.82215766811545,1.,0.171554770204119));
#29873=CARTESIAN_POINT('Ctrl Pts',(-1.80561530629706,1.,0.169936923904608));
#29874=CARTESIAN_POINT('Ctrl Pts',(-1.7869064998507,1.,0.168032772805197));
#29875=CARTESIAN_POINT('Ctrl Pts',(-1.77018771684844,1.,0.1662793551464));
#29876=CARTESIAN_POINT('Ctrl Pts',(-1.75666056638427,1.,0.164834765707158));
#29877=CARTESIAN_POINT('Ctrl Pts',(-1.7472034950333,1.,0.163814161002002));
#29878=CARTESIAN_POINT('Ctrl Pts',(-1.74236521665491,1.,0.163289472382896));
#29879=CARTESIAN_POINT('',(-2.19890268624765,0.,0.069476445021958));
#29880=CARTESIAN_POINT('Origin',(-2.19890268624765,0.,-0.0694764450219585));
#29881=CARTESIAN_POINT('',(-2.19890268624765,1.,-0.0694764450219585));
#29882=CARTESIAN_POINT('',(-2.19890268624765,1.,0.069476445021958));
#29883=CARTESIAN_POINT('',(-2.19890268624765,0.,-0.0694764450219585));
#29884=CARTESIAN_POINT('Ctrl Pts',(-1.74236521665491,-1.,-0.163289472382896));
#29885=CARTESIAN_POINT('Ctrl Pts',(-1.74236521665491,1.,-0.163289472382896));
#29886=CARTESIAN_POINT('Ctrl Pts',(-1.74720349503904,-1.,-0.163814161002474));
#29887=CARTESIAN_POINT('Ctrl Pts',(-1.74720349503904,1.,-0.163814161002474));
#29888=CARTESIAN_POINT('Ctrl Pts',(-1.75666056640041,-1.,-0.164834765708484));
#29889=CARTESIAN_POINT('Ctrl Pts',(-1.75666056640041,1.,-0.164834765708484));
#29890=CARTESIAN_POINT('Ctrl Pts',(-1.77018771687692,-1.,-0.166279355148738));
#29891=CARTESIAN_POINT('Ctrl Pts',(-1.77018771687692,1.,-0.166279355148738));
#29892=CARTESIAN_POINT('Ctrl Pts',(-1.78690649988931,-1.,-0.16803277280837));
#29893=CARTESIAN_POINT('Ctrl Pts',(-1.78690649988931,1.,-0.16803277280837));
#29894=CARTESIAN_POINT('Ctrl Pts',(-1.80561530633924,-1.,-0.169936923908078));
#29895=CARTESIAN_POINT('Ctrl Pts',(-1.80561530633924,1.,-0.169936923908078));
#29896=CARTESIAN_POINT('Ctrl Pts',(-1.82215766815414,-1.,-0.171554770207306));
#29897=CARTESIAN_POINT('Ctrl Pts',(-1.82215766815414,1.,-0.171554770207306));
#29898=CARTESIAN_POINT('Ctrl Pts',(-1.83658380530747,-1.,-0.17288944289442));
#29899=CARTESIAN_POINT('Ctrl Pts',(-1.83658380530747,1.,-0.17288944289442));
#29900=CARTESIAN_POINT('Ctrl Pts',(-1.84898113200543,-1.,-0.173946627589401));
#29901=CARTESIAN_POINT('Ctrl Pts',(-1.84898113200543,1.,-0.173946627589401));
#29902=CARTESIAN_POINT('Ctrl Pts',(-1.85948367089838,-1.,-0.174735259276856));
#29903=CARTESIAN_POINT('Ctrl Pts',(-1.85948367089838,1.,-0.174735259276856));
#29904=CARTESIAN_POINT('Ctrl Pts',(-1.86828349694972,-1.,-0.175268337590901));
#29905=CARTESIAN_POINT('Ctrl Pts',(-1.86828349694972,1.,-0.175268337590901));
#29906=CARTESIAN_POINT('Ctrl Pts',(-1.87563767773249,-1.,-0.175563480746205));
#29907=CARTESIAN_POINT('Ctrl Pts',(-1.87563767773249,1.,-0.175563480746205));
#29908=CARTESIAN_POINT('Ctrl Pts',(-1.88188663144846,-1.,-0.175644148889271));
#29909=CARTESIAN_POINT('Ctrl Pts',(-1.88188663144846,1.,-0.175644148889271));
#29910=CARTESIAN_POINT('Ctrl Pts',(-1.88742606272818,-1.,-0.175538155840286));
#29911=CARTESIAN_POINT('Ctrl Pts',(-1.88742606272818,1.,-0.175538155840286));
#29912=CARTESIAN_POINT('Ctrl Pts',(-1.89264630198279,-1.,-0.175274276190664));
#29913=CARTESIAN_POINT('Ctrl Pts',(-1.89264630198279,1.,-0.175274276190664));
#29914=CARTESIAN_POINT('Ctrl Pts',(-1.89788101117148,-1.,-0.174879405091277));
#29915=CARTESIAN_POINT('Ctrl Pts',(-1.89788101117148,1.,-0.174879405091277));
#29916=CARTESIAN_POINT('Ctrl Pts',(-1.90335253863003,-1.,-0.174375518661222));
#29917=CARTESIAN_POINT('Ctrl Pts',(-1.90335253863003,1.,-0.174375518661222));
#29918=CARTESIAN_POINT('Ctrl Pts',(-1.90911693975475,-1.,-0.173776635257984));
#29919=CARTESIAN_POINT('Ctrl Pts',(-1.90911693975475,1.,-0.173776635257984));
#29920=CARTESIAN_POINT('Ctrl Pts',(-1.91511429159681,-1.,-0.173090695383619));
#29921=CARTESIAN_POINT('Ctrl Pts',(-1.91511429159681,1.,-0.173090695383619));
#29922=CARTESIAN_POINT('Ctrl Pts',(-1.92122334398034,-1.,-0.172321621259557));
#29923=CARTESIAN_POINT('Ctrl Pts',(-1.92122334398034,1.,-0.172321621259557));
#29924=CARTESIAN_POINT('Ctrl Pts',(-1.92731093582,-1.,-0.17147119153296));
#29925=CARTESIAN_POINT('Ctrl Pts',(-1.92731093582,1.,-0.17147119153296));
#29926=CARTESIAN_POINT('Ctrl Pts',(-1.93329183155455,-1.,-0.170541253116136));
#29927=CARTESIAN_POINT('Ctrl Pts',(-1.93329183155455,1.,-0.170541253116136));
#29928=CARTESIAN_POINT('Ctrl Pts',(-1.93915639211497,-1.,-0.169534904817425));
#29929=CARTESIAN_POINT('Ctrl Pts',(-1.93915639211497,1.,-0.169534904817425));
#29930=CARTESIAN_POINT('Ctrl Pts',(-1.94493757756879,-1.,-0.168455741607516));
#29931=CARTESIAN_POINT('Ctrl Pts',(-1.94493757756879,1.,-0.168455741607516));
#29932=CARTESIAN_POINT('Ctrl Pts',(-1.95069027794286,-1.,-0.167307501784469));
#29933=CARTESIAN_POINT('Ctrl Pts',(-1.95069027794286,1.,-0.167307501784469));
#29934=CARTESIAN_POINT('Ctrl Pts',(-1.95646759718755,-1.,-0.166093592002833));
#29935=CARTESIAN_POINT('Ctrl Pts',(-1.95646759718755,1.,-0.166093592002833));
#29936=CARTESIAN_POINT('Ctrl Pts',(-1.96229379940174,-1.,-0.1648165689203));
#29937=CARTESIAN_POINT('Ctrl Pts',(-1.96229379940174,1.,-0.1648165689203));
#29938=CARTESIAN_POINT('Ctrl Pts',(-1.96816512678,-1.,-0.16347818545776));
#29939=CARTESIAN_POINT('Ctrl Pts',(-1.96816512678,1.,-0.16347818545776));
#29940=CARTESIAN_POINT('Ctrl Pts',(-1.97406280235204,-1.,-0.162079693556302));
#29941=CARTESIAN_POINT('Ctrl Pts',(-1.97406280235204,1.,-0.162079693556302));
#29942=CARTESIAN_POINT('Ctrl Pts',(-1.97996195437557,-1.,-0.16062206078461));
#29943=CARTESIAN_POINT('Ctrl Pts',(-1.97996195437557,1.,-0.16062206078461));
#29944=CARTESIAN_POINT('Ctrl Pts',(-1.98584238283279,-1.,-0.159106226437289));
#29945=CARTESIAN_POINT('Ctrl Pts',(-1.98584238283279,1.,-0.159106226437289));
#29946=CARTESIAN_POINT('Ctrl Pts',(-1.99169810931893,-1.,-0.157533331459215));
#29947=CARTESIAN_POINT('Ctrl Pts',(-1.99169810931893,1.,-0.157533331459215));
#29948=CARTESIAN_POINT('Ctrl Pts',(-1.99753284771487,-1.,-0.155904629548775));
#29949=CARTESIAN_POINT('Ctrl Pts',(-1.99753284771487,1.,-0.155904629548775));
#29950=CARTESIAN_POINT('Ctrl Pts',(-2.00335565310539,-1.,-0.154221403049719));
#29951=CARTESIAN_POINT('Ctrl Pts',(-2.00335565310539,1.,-0.154221403049719));
#29952=CARTESIAN_POINT('Ctrl Pts',(-2.00917680318426,-1.,-0.152484883621452));
#29953=CARTESIAN_POINT('Ctrl Pts',(-2.00917680318426,1.,-0.152484883621452));
#29954=CARTESIAN_POINT('Ctrl Pts',(-2.01500291940243,-1.,-0.150696157673084));
#29955=CARTESIAN_POINT('Ctrl Pts',(-2.01500291940243,1.,-0.150696157673084));
#29956=CARTESIAN_POINT('Ctrl Pts',(-2.02083464969897,-1.,-0.148856124775343));
#29957=CARTESIAN_POINT('Ctrl Pts',(-2.02083464969897,1.,-0.148856124775343));
#29958=CARTESIAN_POINT('Ctrl Pts',(-2.02666926182017,-1.,-0.146965557332586));
#29959=CARTESIAN_POINT('Ctrl Pts',(-2.02666926182017,1.,-0.146965557332586));
#29960=CARTESIAN_POINT('Ctrl Pts',(-2.03250223739941,-1.,-0.145025140186058));
#29961=CARTESIAN_POINT('Ctrl Pts',(-2.03250223739941,1.,-0.145025140186058));
#29962=CARTESIAN_POINT('Ctrl Pts',(-2.03832911025913,-1.,-0.143035515058208));
#29963=CARTESIAN_POINT('Ctrl Pts',(-2.03832911025913,1.,-0.143035515058208));
#29964=CARTESIAN_POINT('Ctrl Pts',(-2.04414757947919,-1.,-0.140997332152545));
#29965=CARTESIAN_POINT('Ctrl Pts',(-2.04414757947919,1.,-0.140997332152545));
#29966=CARTESIAN_POINT('Ctrl Pts',(-2.04995762001333,-1.,-0.138911255368966));
#29967=CARTESIAN_POINT('Ctrl Pts',(-2.04995762001333,1.,-0.138911255368966));
#29968=CARTESIAN_POINT('Ctrl Pts',(-2.0557604441427,-1.,-0.136777941218044));
#29969=CARTESIAN_POINT('Ctrl Pts',(-2.0557604441427,1.,-0.136777941218044));
#29970=CARTESIAN_POINT('Ctrl Pts',(-2.06155781517844,-1.,-0.134598026192107));
#29971=CARTESIAN_POINT('Ctrl Pts',(-2.06155781517844,1.,-0.134598026192107));
#29972=CARTESIAN_POINT('Ctrl Pts',(-2.06735123910319,-1.,-0.13237211154771));
#29973=CARTESIAN_POINT('Ctrl Pts',(-2.06735123910319,1.,-0.13237211154771));
#29974=CARTESIAN_POINT('Ctrl Pts',(-2.07314114713047,-1.,-0.130100748328401));
#29975=CARTESIAN_POINT('Ctrl Pts',(-2.07314114713047,1.,-0.130100748328401));
#29976=CARTESIAN_POINT('Ctrl Pts',(-2.07892715110967,-1.,-0.127784445276116));
#29977=CARTESIAN_POINT('Ctrl Pts',(-2.07892715110967,1.,-0.127784445276116));
#29978=CARTESIAN_POINT('Ctrl Pts',(-2.08470840653628,-1.,-0.125423679412058));
#29979=CARTESIAN_POINT('Ctrl Pts',(-2.08470840653628,1.,-0.125423679412058));
#29980=CARTESIAN_POINT('Ctrl Pts',(-2.09048392424826,-1.,-0.123018905621083));
#29981=CARTESIAN_POINT('Ctrl Pts',(-2.09048392424826,1.,-0.123018905621083));
#29982=CARTESIAN_POINT('Ctrl Pts',(-2.09625292867756,-1.,-0.120570567965129));
#29983=CARTESIAN_POINT('Ctrl Pts',(-2.09625292867756,1.,-0.120570567965129));
#29984=CARTESIAN_POINT('Ctrl Pts',(-2.10201512132945,-1.,-0.118079107988368));
#29985=CARTESIAN_POINT('Ctrl Pts',(-2.10201512132945,1.,-0.118079107988368));
#29986=CARTESIAN_POINT('Ctrl Pts',(-2.10777050261359,-1.,-0.11554495768794));
#29987=CARTESIAN_POINT('Ctrl Pts',(-2.10777050261359,1.,-0.11554495768794));
#29988=CARTESIAN_POINT('Ctrl Pts',(-2.11351924490335,-1.,-0.112968534419746));
#29989=CARTESIAN_POINT('Ctrl Pts',(-2.11351924490335,1.,-0.112968534419746));
#29990=CARTESIAN_POINT('Ctrl Pts',(-2.11926155590849,-1.,-0.11035023613502));
#29991=CARTESIAN_POINT('Ctrl Pts',(-2.11926155590849,1.,-0.11035023613502));
#29992=CARTESIAN_POINT('Ctrl Pts',(-2.12499752306927,-1.,-0.107690435231068));
#29993=CARTESIAN_POINT('Ctrl Pts',(-2.12499752306927,1.,-0.107690435231068));
#29994=CARTESIAN_POINT('Ctrl Pts',(-2.1307270488718,-1.,-0.104989479152703));
#29995=CARTESIAN_POINT('Ctrl Pts',(-2.1307270488718,1.,-0.104989479152703));
#29996=CARTESIAN_POINT('Ctrl Pts',(-2.13644992667052,-1.,-0.102247700556064));
#29997=CARTESIAN_POINT('Ctrl Pts',(-2.13644992667052,1.,-0.102247700556064));
#29998=CARTESIAN_POINT('Ctrl Pts',(-2.14216588395974,-1.,-0.0994654261990744));
#29999=CARTESIAN_POINT('Ctrl Pts',(-2.14216588395974,1.,-0.0994654261990744));
#30000=CARTESIAN_POINT('Ctrl Pts',(-2.14787463531864,-1.,-0.096642985230569));
#30001=CARTESIAN_POINT('Ctrl Pts',(-2.14787463531864,1.,-0.096642985230569));
#30002=CARTESIAN_POINT('Ctrl Pts',(-2.15357593978377,-1.,-0.0937807218868346));
#30003=CARTESIAN_POINT('Ctrl Pts',(-2.15357593978377,1.,-0.0937807218868346));
#30004=CARTESIAN_POINT('Ctrl Pts',(-2.15926961544808,-1.,-0.0908789888108267));
#30005=CARTESIAN_POINT('Ctrl Pts',(-2.15926961544808,1.,-0.0908789888108267));
#30006=CARTESIAN_POINT('Ctrl Pts',(-2.16495552645275,-1.,-0.0879381291387824));
#30007=CARTESIAN_POINT('Ctrl Pts',(-2.16495552645275,1.,-0.0879381291387824));
#30008=CARTESIAN_POINT('Ctrl Pts',(-2.17063357871031,-1.,-0.0849584620835644));
#30009=CARTESIAN_POINT('Ctrl Pts',(-2.17063357871031,1.,-0.0849584620835644));
#30010=CARTESIAN_POINT('Ctrl Pts',(-2.1763037121106,-1.,-0.0819402680871941));
#30011=CARTESIAN_POINT('Ctrl Pts',(-2.1763037121106,1.,-0.0819402680871941));
#30012=CARTESIAN_POINT('Ctrl Pts',(-2.18196589448304,-1.,-0.0788837727683229));
#30013=CARTESIAN_POINT('Ctrl Pts',(-2.18196589448304,1.,-0.0788837727683229));
#30014=CARTESIAN_POINT('Ctrl Pts',(-2.1876201139874,-1.,-0.0757891465833413));
#30015=CARTESIAN_POINT('Ctrl Pts',(-2.1876201139874,1.,-0.0757891465833413));
#30016=CARTESIAN_POINT('Ctrl Pts',(-2.19213712012956,-1.,-0.0732830357304277));
#30017=CARTESIAN_POINT('Ctrl Pts',(-2.19213712012956,1.,-0.0732830357304277));
#30018=CARTESIAN_POINT('Ctrl Pts',(-2.19552129483562,-1.,-0.0713863779524629));
#30019=CARTESIAN_POINT('Ctrl Pts',(-2.19552129483562,1.,-0.0713863779524629));
#30020=CARTESIAN_POINT('Ctrl Pts',(-2.19777582085261,-1.,-0.0701143536324927));
#30021=CARTESIAN_POINT('Ctrl Pts',(-2.19777582085261,1.,-0.0701143536324927));
#30022=CARTESIAN_POINT('Ctrl Pts',(-2.19890268624765,-1.,-0.0694764450219585));
#30023=CARTESIAN_POINT('Ctrl Pts',(-2.19890268624765,1.,-0.0694764450219585));
#30024=CARTESIAN_POINT('',(-1.74236521665491,1.,-0.163289472382896));
#30025=CARTESIAN_POINT('Ctrl Pts',(-1.74236521665491,1.,-0.163289472382896));
#30026=CARTESIAN_POINT('Ctrl Pts',(-1.74720349503904,1.,-0.163814161002474));
#30027=CARTESIAN_POINT('Ctrl Pts',(-1.75666056640041,1.,-0.164834765708484));
#30028=CARTESIAN_POINT('Ctrl Pts',(-1.77018771687692,1.,-0.166279355148738));
#30029=CARTESIAN_POINT('Ctrl Pts',(-1.78690649988931,1.,-0.16803277280837));
#30030=CARTESIAN_POINT('Ctrl Pts',(-1.80561530633924,1.,-0.169936923908078));
#30031=CARTESIAN_POINT('Ctrl Pts',(-1.82215766815414,1.,-0.171554770207306));
#30032=CARTESIAN_POINT('Ctrl Pts',(-1.83658380530747,1.,-0.17288944289442));
#30033=CARTESIAN_POINT('Ctrl Pts',(-1.84898113200543,1.,-0.173946627589401));
#30034=CARTESIAN_POINT('Ctrl Pts',(-1.85948367089838,1.,-0.174735259276856));
#30035=CARTESIAN_POINT('Ctrl Pts',(-1.86828349694972,1.,-0.175268337590901));
#30036=CARTESIAN_POINT('Ctrl Pts',(-1.87563767773249,1.,-0.175563480746205));
#30037=CARTESIAN_POINT('Ctrl Pts',(-1.88188663144846,1.,-0.175644148889271));
#30038=CARTESIAN_POINT('Ctrl Pts',(-1.88742606272818,1.,-0.175538155840286));
#30039=CARTESIAN_POINT('Ctrl Pts',(-1.89264630198279,1.,-0.175274276190664));
#30040=CARTESIAN_POINT('Ctrl Pts',(-1.89788101117148,1.,-0.174879405091277));
#30041=CARTESIAN_POINT('Ctrl Pts',(-1.90335253863003,1.,-0.174375518661222));
#30042=CARTESIAN_POINT('Ctrl Pts',(-1.90911693975475,1.,-0.173776635257984));
#30043=CARTESIAN_POINT('Ctrl Pts',(-1.91511429159681,1.,-0.173090695383619));
#30044=CARTESIAN_POINT('Ctrl Pts',(-1.92122334398034,1.,-0.172321621259557));
#30045=CARTESIAN_POINT('Ctrl Pts',(-1.92731093582,1.,-0.17147119153296));
#30046=CARTESIAN_POINT('Ctrl Pts',(-1.93329183155455,1.,-0.170541253116136));
#30047=CARTESIAN_POINT('Ctrl Pts',(-1.93915639211497,1.,-0.169534904817425));
#30048=CARTESIAN_POINT('Ctrl Pts',(-1.94493757756879,1.,-0.168455741607516));
#30049=CARTESIAN_POINT('Ctrl Pts',(-1.95069027794286,1.,-0.167307501784469));
#30050=CARTESIAN_POINT('Ctrl Pts',(-1.95646759718755,1.,-0.166093592002833));
#30051=CARTESIAN_POINT('Ctrl Pts',(-1.96229379940174,1.,-0.1648165689203));
#30052=CARTESIAN_POINT('Ctrl Pts',(-1.96816512678,1.,-0.16347818545776));
#30053=CARTESIAN_POINT('Ctrl Pts',(-1.97406280235204,1.,-0.162079693556302));
#30054=CARTESIAN_POINT('Ctrl Pts',(-1.97996195437557,1.,-0.16062206078461));
#30055=CARTESIAN_POINT('Ctrl Pts',(-1.98584238283279,1.,-0.159106226437289));
#30056=CARTESIAN_POINT('Ctrl Pts',(-1.99169810931893,1.,-0.157533331459215));
#30057=CARTESIAN_POINT('Ctrl Pts',(-1.99753284771487,1.,-0.155904629548775));
#30058=CARTESIAN_POINT('Ctrl Pts',(-2.00335565310539,1.,-0.154221403049719));
#30059=CARTESIAN_POINT('Ctrl Pts',(-2.00917680318426,1.,-0.152484883621452));
#30060=CARTESIAN_POINT('Ctrl Pts',(-2.01500291940243,1.,-0.150696157673084));
#30061=CARTESIAN_POINT('Ctrl Pts',(-2.02083464969897,1.,-0.148856124775343));
#30062=CARTESIAN_POINT('Ctrl Pts',(-2.02666926182017,1.,-0.146965557332586));
#30063=CARTESIAN_POINT('Ctrl Pts',(-2.03250223739941,1.,-0.145025140186058));
#30064=CARTESIAN_POINT('Ctrl Pts',(-2.03832911025913,1.,-0.143035515058208));
#30065=CARTESIAN_POINT('Ctrl Pts',(-2.04414757947919,1.,-0.140997332152545));
#30066=CARTESIAN_POINT('Ctrl Pts',(-2.04995762001333,1.,-0.138911255368966));
#30067=CARTESIAN_POINT('Ctrl Pts',(-2.0557604441427,1.,-0.136777941218044));
#30068=CARTESIAN_POINT('Ctrl Pts',(-2.06155781517844,1.,-0.134598026192107));
#30069=CARTESIAN_POINT('Ctrl Pts',(-2.06735123910319,1.,-0.13237211154771));
#30070=CARTESIAN_POINT('Ctrl Pts',(-2.07314114713047,1.,-0.130100748328401));
#30071=CARTESIAN_POINT('Ctrl Pts',(-2.07892715110967,1.,-0.127784445276116));
#30072=CARTESIAN_POINT('Ctrl Pts',(-2.08470840653628,1.,-0.125423679412058));
#30073=CARTESIAN_POINT('Ctrl Pts',(-2.09048392424826,1.,-0.123018905621083));
#30074=CARTESIAN_POINT('Ctrl Pts',(-2.09625292867756,1.,-0.120570567965129));
#30075=CARTESIAN_POINT('Ctrl Pts',(-2.10201512132945,1.,-0.118079107988368));
#30076=CARTESIAN_POINT('Ctrl Pts',(-2.10777050261359,1.,-0.11554495768794));
#30077=CARTESIAN_POINT('Ctrl Pts',(-2.11351924490335,1.,-0.112968534419746));
#30078=CARTESIAN_POINT('Ctrl Pts',(-2.11926155590849,1.,-0.11035023613502));
#30079=CARTESIAN_POINT('Ctrl Pts',(-2.12499752306927,1.,-0.107690435231068));
#30080=CARTESIAN_POINT('Ctrl Pts',(-2.1307270488718,1.,-0.104989479152703));
#30081=CARTESIAN_POINT('Ctrl Pts',(-2.13644992667052,1.,-0.102247700556064));
#30082=CARTESIAN_POINT('Ctrl Pts',(-2.14216588395974,1.,-0.0994654261990744));
#30083=CARTESIAN_POINT('Ctrl Pts',(-2.14787463531864,1.,-0.096642985230569));
#30084=CARTESIAN_POINT('Ctrl Pts',(-2.15357593978377,1.,-0.0937807218868346));
#30085=CARTESIAN_POINT('Ctrl Pts',(-2.15926961544808,1.,-0.0908789888108267));
#30086=CARTESIAN_POINT('Ctrl Pts',(-2.16495552645275,1.,-0.0879381291387824));
#30087=CARTESIAN_POINT('Ctrl Pts',(-2.17063357871031,1.,-0.0849584620835644));
#30088=CARTESIAN_POINT('Ctrl Pts',(-2.1763037121106,1.,-0.0819402680871941));
#30089=CARTESIAN_POINT('Ctrl Pts',(-2.18196589448304,1.,-0.0788837727683229));
#30090=CARTESIAN_POINT('Ctrl Pts',(-2.1876201139874,1.,-0.0757891465833413));
#30091=CARTESIAN_POINT('Ctrl Pts',(-2.19213712012956,1.,-0.0732830357304277));
#30092=CARTESIAN_POINT('Ctrl Pts',(-2.19552129483562,1.,-0.0713863779524629));
#30093=CARTESIAN_POINT('Ctrl Pts',(-2.19777582085261,1.,-0.0701143536324927));
#30094=CARTESIAN_POINT('Ctrl Pts',(-2.19890268624765,1.,-0.0694764450219585));
#30095=CARTESIAN_POINT('',(-1.74236521665491,0.,-0.163289472382896));
#30096=CARTESIAN_POINT('Origin',(0.,0.,0.));
#30097=CARTESIAN_POINT('',(-1.7075470150345,1.,-0.383122945602004));
#30098=CARTESIAN_POINT('Origin',(0.,1.,0.));
#30099=CARTESIAN_POINT('',(-1.7075470150345,0.,-0.383122945602004));
#30100=CARTESIAN_POINT('Ctrl Pts',(-2.11275013067528,-1.,-0.61342227326009));
#30101=CARTESIAN_POINT('Ctrl Pts',(-2.11275013067528,1.,-0.61342227326009));
#30102=CARTESIAN_POINT('Ctrl Pts',(-2.11187554260142,-1.,-0.61246736556225));
#30103=CARTESIAN_POINT('Ctrl Pts',(-2.11187554260142,1.,-0.61246736556225));
#30104=CARTESIAN_POINT('Ctrl Pts',(-2.11012443807661,-1.,-0.610560911691113));
#30105=CARTESIAN_POINT('Ctrl Pts',(-2.11012443807661,1.,-0.610560911691113));
#30106=CARTESIAN_POINT('Ctrl Pts',(-2.10749199615859,-1.,-0.607711315456826));
#30107=CARTESIAN_POINT('Ctrl Pts',(-2.10749199615859,1.,-0.607711315456826));
#30108=CARTESIAN_POINT('Ctrl Pts',(-2.10397049887709,-1.,-0.603932030738212));
#30109=CARTESIAN_POINT('Ctrl Pts',(-2.10397049887709,1.,-0.603932030738212));
#30110=CARTESIAN_POINT('Ctrl Pts',(-2.09954930865331,-1.,-0.599241616422144));
#30111=CARTESIAN_POINT('Ctrl Pts',(-2.09954930865331,1.,-0.599241616422144));
#30112=CARTESIAN_POINT('Ctrl Pts',(-2.09510876220501,-1.,-0.594585006052823));
#30113=CARTESIAN_POINT('Ctrl Pts',(-2.09510876220501,1.,-0.594585006052823));
#30114=CARTESIAN_POINT('Ctrl Pts',(-2.09064881812053,-1.,-0.589962365403189));
#30115=CARTESIAN_POINT('Ctrl Pts',(-2.09064881812053,1.,-0.589962365403189));
#30116=CARTESIAN_POINT('Ctrl Pts',(-2.086169437277,-1.,-0.585373918990895));
#30117=CARTESIAN_POINT('Ctrl Pts',(-2.086169437277,1.,-0.585373918990895));
#30118=CARTESIAN_POINT('Ctrl Pts',(-2.08167059018138,-1.,-0.580819952107257));
#30119=CARTESIAN_POINT('Ctrl Pts',(-2.08167059018138,1.,-0.580819952107257));
#30120=CARTESIAN_POINT('Ctrl Pts',(-2.07715226767361,-1.,-0.576300797416274));
#30121=CARTESIAN_POINT('Ctrl Pts',(-2.07715226767361,1.,-0.576300797416274));
#30122=CARTESIAN_POINT('Ctrl Pts',(-2.07261449292757,-1.,-0.571816823242411));
#30123=CARTESIAN_POINT('Ctrl Pts',(-2.07261449292757,1.,-0.571816823242411));
#30124=CARTESIAN_POINT('Ctrl Pts',(-2.06805732997383,-1.,-0.567368421181229));
#30125=CARTESIAN_POINT('Ctrl Pts',(-2.06805732997383,1.,-0.567368421181229));
#30126=CARTESIAN_POINT('Ctrl Pts',(-2.06348090160697,-1.,-0.562955993082574));
#30127=CARTESIAN_POINT('Ctrl Pts',(-2.06348090160697,1.,-0.562955993082574));
#30128=CARTESIAN_POINT('Ctrl Pts',(-2.05888537756571,-1.,-0.558579940185467));
#30129=CARTESIAN_POINT('Ctrl Pts',(-2.05888537756571,1.,-0.558579940185467));
#30130=CARTESIAN_POINT('Ctrl Pts',(-2.05427091604482,-1.,-0.554240657464109));
#30131=CARTESIAN_POINT('Ctrl Pts',(-2.05427091604482,1.,-0.554240657464109));
#30132=CARTESIAN_POINT('Ctrl Pts',(-2.04963761077974,-1.,-0.549938525150342));
#30133=CARTESIAN_POINT('Ctrl Pts',(-2.04963761077974,1.,-0.549938525150342));
#30134=CARTESIAN_POINT('Ctrl Pts',(-2.0449854471456,-1.,-0.545673903817348));
#30135=CARTESIAN_POINT('Ctrl Pts',(-2.0449854471456,1.,-0.545673903817348));
#30136=CARTESIAN_POINT('Ctrl Pts',(-2.0403142269048,-1.,-0.54144712061552));
#30137=CARTESIAN_POINT('Ctrl Pts',(-2.0403142269048,1.,-0.54144712061552));
#30138=CARTESIAN_POINT('Ctrl Pts',(-2.03562362953993,-1.,-0.537258489833134));
#30139=CARTESIAN_POINT('Ctrl Pts',(-2.03562362953993,1.,-0.537258489833134));
#30140=CARTESIAN_POINT('Ctrl Pts',(-2.03091336214401,-1.,-0.533108355132905));
#30141=CARTESIAN_POINT('Ctrl Pts',(-2.03091336214401,1.,-0.533108355132905));
#30142=CARTESIAN_POINT('Ctrl Pts',(-2.02618329083289,-1.,-0.52899712724191));
#30143=CARTESIAN_POINT('Ctrl Pts',(-2.02618329083289,1.,-0.52899712724191));
#30144=CARTESIAN_POINT('Ctrl Pts',(-2.02143356304712,-1.,-0.524925318333518));
#30145=CARTESIAN_POINT('Ctrl Pts',(-2.02143356304712,1.,-0.524925318333518));
#30146=CARTESIAN_POINT('Ctrl Pts',(-2.01666477917305,-1.,-0.520893590399428));
#30147=CARTESIAN_POINT('Ctrl Pts',(-2.01666477917305,1.,-0.520893590399428));
#30148=CARTESIAN_POINT('Ctrl Pts',(-2.01187773939257,-1.,-0.516902681728733));
#30149=CARTESIAN_POINT('Ctrl Pts',(-2.01187773939257,1.,-0.516902681728733));
#30150=CARTESIAN_POINT('Ctrl Pts',(-2.00707309946955,-1.,-0.512953306961813));
#30151=CARTESIAN_POINT('Ctrl Pts',(-2.00707309946955,1.,-0.512953306961813));
#30152=CARTESIAN_POINT('Ctrl Pts',(-2.00225107134733,-1.,-0.509046069886152));
#30153=CARTESIAN_POINT('Ctrl Pts',(-2.00225107134733,1.,-0.509046069886152));
#30154=CARTESIAN_POINT('Ctrl Pts',(-1.99741107463567,-1.,-0.505181361323011));
#30155=CARTESIAN_POINT('Ctrl Pts',(-1.99741107463567,1.,-0.505181361323011));
#30156=CARTESIAN_POINT('Ctrl Pts',(-1.9925514912615,-1.,-0.501359287727129));
#30157=CARTESIAN_POINT('Ctrl Pts',(-1.9925514912615,1.,-0.501359287727129));
#30158=CARTESIAN_POINT('Ctrl Pts',(-1.98767044752929,-1.,-0.497579909545564));
#30159=CARTESIAN_POINT('Ctrl Pts',(-1.98767044752929,1.,-0.497579909545564));
#30160=CARTESIAN_POINT('Ctrl Pts',(-1.9827665876182,-1.,-0.493843476541492));
#30161=CARTESIAN_POINT('Ctrl Pts',(-1.9827665876182,1.,-0.493843476541492));
#30162=CARTESIAN_POINT('Ctrl Pts',(-1.97783973019229,-1.,-0.490150627860955));
#30163=CARTESIAN_POINT('Ctrl Pts',(-1.97783973019229,1.,-0.490150627860955));
#30164=CARTESIAN_POINT('Ctrl Pts',(-1.97289186263272,-1.,-0.486502692907661));
#30165=CARTESIAN_POINT('Ctrl Pts',(-1.97289186263272,1.,-0.486502692907661));
#30166=CARTESIAN_POINT('Ctrl Pts',(-1.96792703422358,-1.,-0.482901662120686));
#30167=CARTESIAN_POINT('Ctrl Pts',(-1.96792703422358,1.,-0.482901662120686));
#30168=CARTESIAN_POINT('Ctrl Pts',(-1.96294933055938,-1.,-0.479349583074846));
#30169=CARTESIAN_POINT('Ctrl Pts',(-1.96294933055938,1.,-0.479349583074846));
#30170=CARTESIAN_POINT('Ctrl Pts',(-1.95796111148175,-1.,-0.475848034683171));
#30171=CARTESIAN_POINT('Ctrl Pts',(-1.95796111148175,1.,-0.475848034683171));
#30172=CARTESIAN_POINT('Ctrl Pts',(-1.95296148278136,-1.,-0.472397672264079));
#30173=CARTESIAN_POINT('Ctrl Pts',(-1.95296148278136,1.,-0.472397672264079));
#30174=CARTESIAN_POINT('Ctrl Pts',(-1.94794381136524,-1.,-0.468997482913158));
#30175=CARTESIAN_POINT('Ctrl Pts',(-1.94794381136524,1.,-0.468997482913158));
#30176=CARTESIAN_POINT('Ctrl Pts',(-1.94289794196205,-1.,-0.465645462026064));
#30177=CARTESIAN_POINT('Ctrl Pts',(-1.94289794196205,1.,-0.465645462026064));
#30178=CARTESIAN_POINT('Ctrl Pts',(-1.93781486640834,-1.,-0.462340031009087));
#30179=CARTESIAN_POINT('Ctrl Pts',(-1.93781486640834,1.,-0.462340031009087));
#30180=CARTESIAN_POINT('Ctrl Pts',(-1.93269066517936,-1.,-0.459081234547931));
#30181=CARTESIAN_POINT('Ctrl Pts',(-1.93269066517936,1.,-0.459081234547931));
#30182=CARTESIAN_POINT('Ctrl Pts',(-1.92753067150461,-1.,-0.455872005174335));
#30183=CARTESIAN_POINT('Ctrl Pts',(-1.92753067150461,1.,-0.455872005174335));
#30184=CARTESIAN_POINT('Ctrl Pts',(-1.9223538064847,-1.,-0.452719478359356));
#30185=CARTESIAN_POINT('Ctrl Pts',(-1.9223538064847,1.,-0.452719478359356));
#30186=CARTESIAN_POINT('Ctrl Pts',(-1.91718342555717,-1.,-0.449632260106572));
#30187=CARTESIAN_POINT('Ctrl Pts',(-1.91718342555717,1.,-0.449632260106572));
#30188=CARTESIAN_POINT('Ctrl Pts',(-1.91203699981095,-1.,-0.446617343485651));
#30189=CARTESIAN_POINT('Ctrl Pts',(-1.91203699981095,1.,-0.446617343485651));
#30190=CARTESIAN_POINT('Ctrl Pts',(-1.90691756144906,-1.,-0.44367755684917));
#30191=CARTESIAN_POINT('Ctrl Pts',(-1.90691756144906,1.,-0.44367755684917));
#30192=CARTESIAN_POINT('Ctrl Pts',(-1.90180124389137,-1.,-0.44080783370416));
#30193=CARTESIAN_POINT('Ctrl Pts',(-1.90180124389137,1.,-0.44080783370416));
#30194=CARTESIAN_POINT('Ctrl Pts',(-1.89663648956549,-1.,-0.437995003948443));
#30195=CARTESIAN_POINT('Ctrl Pts',(-1.89663648956549,1.,-0.437995003948443));
#30196=CARTESIAN_POINT('Ctrl Pts',(-1.89136993975585,-1.,-0.43522566096358));
#30197=CARTESIAN_POINT('Ctrl Pts',(-1.89136993975585,1.,-0.43522566096358));
#30198=CARTESIAN_POINT('Ctrl Pts',(-1.88596913666828,-1.,-0.432493038548833));
#30199=CARTESIAN_POINT('Ctrl Pts',(-1.88596913666828,1.,-0.432493038548833));
#30200=CARTESIAN_POINT('Ctrl Pts',(-1.88044229001778,-1.,-0.429803062482217));
#30201=CARTESIAN_POINT('Ctrl Pts',(-1.88044229001778,1.,-0.429803062482217));
#30202=CARTESIAN_POINT('Ctrl Pts',(-1.87486989291333,-1.,-0.427183828518743));
#30203=CARTESIAN_POINT('Ctrl Pts',(-1.87486989291333,1.,-0.427183828518743));
#30204=CARTESIAN_POINT('Ctrl Pts',(-1.8693780394412,-1.,-0.424678177290876));
#30205=CARTESIAN_POINT('Ctrl Pts',(-1.8693780394412,1.,-0.424678177290876));
#30206=CARTESIAN_POINT('Ctrl Pts',(-1.86408083333863,-1.,-0.422327307417884));
#30207=CARTESIAN_POINT('Ctrl Pts',(-1.86408083333863,1.,-0.422327307417884));
#30208=CARTESIAN_POINT('Ctrl Pts',(-1.8590328109667,-1.,-0.420157287975583));
#30209=CARTESIAN_POINT('Ctrl Pts',(-1.8590328109667,1.,-0.420157287975583));
#30210=CARTESIAN_POINT('Ctrl Pts',(-1.8541763285645,-1.,-0.418164129144045));
#30211=CARTESIAN_POINT('Ctrl Pts',(-1.8541763285645,1.,-0.418164129144045));
#30212=CARTESIAN_POINT('Ctrl Pts',(-1.84929312930314,-1.,-0.416300022039885));
#30213=CARTESIAN_POINT('Ctrl Pts',(-1.84929312930314,1.,-0.416300022039885));
#30214=CARTESIAN_POINT('Ctrl Pts',(-1.84405757074218,-1.,-0.414487438255542));
#30215=CARTESIAN_POINT('Ctrl Pts',(-1.84405757074218,1.,-0.414487438255542));
#30216=CARTESIAN_POINT('Ctrl Pts',(-1.8380895347617,-1.,-0.412633125322945));
#30217=CARTESIAN_POINT('Ctrl Pts',(-1.8380895347617,1.,-0.412633125322945));
#30218=CARTESIAN_POINT('Ctrl Pts',(-1.83100408895047,-1.,-0.410641256301276));
#30219=CARTESIAN_POINT('Ctrl Pts',(-1.83100408895047,1.,-0.410641256301276));
#30220=CARTESIAN_POINT('Ctrl Pts',(-1.82247022677562,-1.,-0.408428948106227));
#30221=CARTESIAN_POINT('Ctrl Pts',(-1.82247022677562,1.,-0.408428948106227));
#30222=CARTESIAN_POINT('Ctrl Pts',(-1.81223801812013,-1.,-0.405933518407175));
#30223=CARTESIAN_POINT('Ctrl Pts',(-1.81223801812013,1.,-0.405933518407175));
#30224=CARTESIAN_POINT('Ctrl Pts',(-1.80012077173238,-1.,-0.403107976163396));
#30225=CARTESIAN_POINT('Ctrl Pts',(-1.80012077173238,1.,-0.403107976163396));
#30226=CARTESIAN_POINT('Ctrl Pts',(-1.78598826343754,-1.,-0.399919403774155));
#30227=CARTESIAN_POINT('Ctrl Pts',(-1.78598826343754,1.,-0.399919403774155));
#30228=CARTESIAN_POINT('Ctrl Pts',(-1.76975560043442,-1.,-0.396346196110688));
#30229=CARTESIAN_POINT('Ctrl Pts',(-1.76975560043442,1.,-0.396346196110688));
#30230=CARTESIAN_POINT('Ctrl Pts',(-1.75137405310193,-1.,-0.392375812285395));
#30231=CARTESIAN_POINT('Ctrl Pts',(-1.75137405310193,1.,-0.392375812285395));
#30232=CARTESIAN_POINT('Ctrl Pts',(-1.73493170972829,-1.,-0.388877023502615));
#30233=CARTESIAN_POINT('Ctrl Pts',(-1.73493170972829,1.,-0.388877023502615));
#30234=CARTESIAN_POINT('Ctrl Pts',(-1.72162022244582,-1.,-0.386070790323281));
#30235=CARTESIAN_POINT('Ctrl Pts',(-1.72162022244582,1.,-0.386070790323281));
#30236=CARTESIAN_POINT('Ctrl Pts',(-1.71231062891398,-1.,-0.384119047314215));
#30237=CARTESIAN_POINT('Ctrl Pts',(-1.71231062891398,1.,-0.384119047314215));
#30238=CARTESIAN_POINT('Ctrl Pts',(-1.7075470150345,-1.,-0.383122945602004));
#30239=CARTESIAN_POINT('Ctrl Pts',(-1.7075470150345,1.,-0.383122945602004));
#30240=CARTESIAN_POINT('',(-2.11275013067528,1.,-0.61342227326009));
#30241=CARTESIAN_POINT('Ctrl Pts',(-2.11275013067528,1.,-0.61342227326009));
#30242=CARTESIAN_POINT('Ctrl Pts',(-2.11187554260142,1.,-0.61246736556225));
#30243=CARTESIAN_POINT('Ctrl Pts',(-2.11012443807661,1.,-0.610560911691113));
#30244=CARTESIAN_POINT('Ctrl Pts',(-2.10749199615859,1.,-0.607711315456826));
#30245=CARTESIAN_POINT('Ctrl Pts',(-2.10397049887709,1.,-0.603932030738212));
#30246=CARTESIAN_POINT('Ctrl Pts',(-2.09954930865331,1.,-0.599241616422144));
#30247=CARTESIAN_POINT('Ctrl Pts',(-2.09510876220501,1.,-0.594585006052823));
#30248=CARTESIAN_POINT('Ctrl Pts',(-2.09064881812053,1.,-0.589962365403189));
#30249=CARTESIAN_POINT('Ctrl Pts',(-2.086169437277,1.,-0.585373918990895));
#30250=CARTESIAN_POINT('Ctrl Pts',(-2.08167059018138,1.,-0.580819952107257));
#30251=CARTESIAN_POINT('Ctrl Pts',(-2.07715226767361,1.,-0.576300797416274));
#30252=CARTESIAN_POINT('Ctrl Pts',(-2.07261449292757,1.,-0.571816823242411));
#30253=CARTESIAN_POINT('Ctrl Pts',(-2.06805732997383,1.,-0.567368421181229));
#30254=CARTESIAN_POINT('Ctrl Pts',(-2.06348090160697,1.,-0.562955993082574));
#30255=CARTESIAN_POINT('Ctrl Pts',(-2.05888537756571,1.,-0.558579940185467));
#30256=CARTESIAN_POINT('Ctrl Pts',(-2.05427091604482,1.,-0.554240657464109));
#30257=CARTESIAN_POINT('Ctrl Pts',(-2.04963761077974,1.,-0.549938525150342));
#30258=CARTESIAN_POINT('Ctrl Pts',(-2.0449854471456,1.,-0.545673903817348));
#30259=CARTESIAN_POINT('Ctrl Pts',(-2.0403142269048,1.,-0.54144712061552));
#30260=CARTESIAN_POINT('Ctrl Pts',(-2.03562362953993,1.,-0.537258489833134));
#30261=CARTESIAN_POINT('Ctrl Pts',(-2.03091336214401,1.,-0.533108355132905));
#30262=CARTESIAN_POINT('Ctrl Pts',(-2.02618329083289,1.,-0.52899712724191));
#30263=CARTESIAN_POINT('Ctrl Pts',(-2.02143356304712,1.,-0.524925318333518));
#30264=CARTESIAN_POINT('Ctrl Pts',(-2.01666477917305,1.,-0.520893590399428));
#30265=CARTESIAN_POINT('Ctrl Pts',(-2.01187773939257,1.,-0.516902681728733));
#30266=CARTESIAN_POINT('Ctrl Pts',(-2.00707309946955,1.,-0.512953306961813));
#30267=CARTESIAN_POINT('Ctrl Pts',(-2.00225107134733,1.,-0.509046069886152));
#30268=CARTESIAN_POINT('Ctrl Pts',(-1.99741107463567,1.,-0.505181361323011));
#30269=CARTESIAN_POINT('Ctrl Pts',(-1.9925514912615,1.,-0.501359287727129));
#30270=CARTESIAN_POINT('Ctrl Pts',(-1.98767044752929,1.,-0.497579909545564));
#30271=CARTESIAN_POINT('Ctrl Pts',(-1.9827665876182,1.,-0.493843476541492));
#30272=CARTESIAN_POINT('Ctrl Pts',(-1.97783973019229,1.,-0.490150627860955));
#30273=CARTESIAN_POINT('Ctrl Pts',(-1.97289186263272,1.,-0.486502692907661));
#30274=CARTESIAN_POINT('Ctrl Pts',(-1.96792703422358,1.,-0.482901662120686));
#30275=CARTESIAN_POINT('Ctrl Pts',(-1.96294933055938,1.,-0.479349583074846));
#30276=CARTESIAN_POINT('Ctrl Pts',(-1.95796111148175,1.,-0.475848034683171));
#30277=CARTESIAN_POINT('Ctrl Pts',(-1.95296148278136,1.,-0.472397672264079));
#30278=CARTESIAN_POINT('Ctrl Pts',(-1.94794381136524,1.,-0.468997482913158));
#30279=CARTESIAN_POINT('Ctrl Pts',(-1.94289794196205,1.,-0.465645462026064));
#30280=CARTESIAN_POINT('Ctrl Pts',(-1.93781486640834,1.,-0.462340031009087));
#30281=CARTESIAN_POINT('Ctrl Pts',(-1.93269066517936,1.,-0.459081234547931));
#30282=CARTESIAN_POINT('Ctrl Pts',(-1.92753067150461,1.,-0.455872005174335));
#30283=CARTESIAN_POINT('Ctrl Pts',(-1.9223538064847,1.,-0.452719478359356));
#30284=CARTESIAN_POINT('Ctrl Pts',(-1.91718342555717,1.,-0.449632260106572));
#30285=CARTESIAN_POINT('Ctrl Pts',(-1.91203699981095,1.,-0.446617343485651));
#30286=CARTESIAN_POINT('Ctrl Pts',(-1.90691756144906,1.,-0.44367755684917));
#30287=CARTESIAN_POINT('Ctrl Pts',(-1.90180124389137,1.,-0.44080783370416));
#30288=CARTESIAN_POINT('Ctrl Pts',(-1.89663648956549,1.,-0.437995003948443));
#30289=CARTESIAN_POINT('Ctrl Pts',(-1.89136993975585,1.,-0.43522566096358));
#30290=CARTESIAN_POINT('Ctrl Pts',(-1.88596913666828,1.,-0.432493038548833));
#30291=CARTESIAN_POINT('Ctrl Pts',(-1.88044229001778,1.,-0.429803062482217));
#30292=CARTESIAN_POINT('Ctrl Pts',(-1.87486989291333,1.,-0.427183828518743));
#30293=CARTESIAN_POINT('Ctrl Pts',(-1.8693780394412,1.,-0.424678177290876));
#30294=CARTESIAN_POINT('Ctrl Pts',(-1.86408083333863,1.,-0.422327307417884));
#30295=CARTESIAN_POINT('Ctrl Pts',(-1.8590328109667,1.,-0.420157287975583));
#30296=CARTESIAN_POINT('Ctrl Pts',(-1.8541763285645,1.,-0.418164129144045));
#30297=CARTESIAN_POINT('Ctrl Pts',(-1.84929312930314,1.,-0.416300022039885));
#30298=CARTESIAN_POINT('Ctrl Pts',(-1.84405757074218,1.,-0.414487438255542));
#30299=CARTESIAN_POINT('Ctrl Pts',(-1.8380895347617,1.,-0.412633125322945));
#30300=CARTESIAN_POINT('Ctrl Pts',(-1.83100408895047,1.,-0.410641256301276));
#30301=CARTESIAN_POINT('Ctrl Pts',(-1.82247022677562,1.,-0.408428948106227));
#30302=CARTESIAN_POINT('Ctrl Pts',(-1.81223801812013,1.,-0.405933518407175));
#30303=CARTESIAN_POINT('Ctrl Pts',(-1.80012077173238,1.,-0.403107976163396));
#30304=CARTESIAN_POINT('Ctrl Pts',(-1.78598826343754,1.,-0.399919403774155));
#30305=CARTESIAN_POINT('Ctrl Pts',(-1.76975560043442,1.,-0.396346196110688));
#30306=CARTESIAN_POINT('Ctrl Pts',(-1.75137405310193,1.,-0.392375812285395));
#30307=CARTESIAN_POINT('Ctrl Pts',(-1.73493170972829,1.,-0.388877023502615));
#30308=CARTESIAN_POINT('Ctrl Pts',(-1.72162022244582,1.,-0.386070790323281));
#30309=CARTESIAN_POINT('Ctrl Pts',(-1.71231062891398,1.,-0.384119047314215));
#30310=CARTESIAN_POINT('Ctrl Pts',(-1.7075470150345,1.,-0.383122945602004));
#30311=CARTESIAN_POINT('',(-2.11275013067528,0.,-0.61342227326009));
#30312=CARTESIAN_POINT('Origin',(-2.0698113262342,0.,-0.745574324794401));
#30313=CARTESIAN_POINT('',(-2.0698113262342,1.,-0.745574324794401));
#30314=CARTESIAN_POINT('',(-2.11275013067528,1.,-0.61342227326009));
#30315=CARTESIAN_POINT('',(-2.0698113262342,0.,-0.745574324794401));
#30316=CARTESIAN_POINT('Ctrl Pts',(-1.60662857109684,-1.,-0.693717979106306));
#30317=CARTESIAN_POINT('Ctrl Pts',(-1.60662857109684,1.,-0.693717979106306));
#30318=CARTESIAN_POINT('Ctrl Pts',(-1.61106790958151,-1.,-0.695712097881194));
#30319=CARTESIAN_POINT('Ctrl Pts',(-1.61106790958151,1.,-0.695712097881194));
#30320=CARTESIAN_POINT('Ctrl Pts',(-1.61974673472612,-1.,-0.699605146405088));
#30321=CARTESIAN_POINT('Ctrl Pts',(-1.61974673472612,1.,-0.699605146405088));
#30322=CARTESIAN_POINT('Ctrl Pts',(-1.63216541664676,-1.,-0.705159151988319));
#30323=CARTESIAN_POINT('Ctrl Pts',(-1.63216541664676,1.,-0.705159151988319));
#30324=CARTESIAN_POINT('Ctrl Pts',(-1.64752408832016,-1.,-0.711993139355394));
#30325=CARTESIAN_POINT('Ctrl Pts',(-1.64752408832016,1.,-0.711993139355394));
#30326=CARTESIAN_POINT('Ctrl Pts',(-1.6647288055568,-1.,-0.719585433804282));
#30327=CARTESIAN_POINT('Ctrl Pts',(-1.6647288055568,1.,-0.719585433804282));
#30328=CARTESIAN_POINT('Ctrl Pts',(-1.67996158455503,-1.,-0.726235967997433));
#30329=CARTESIAN_POINT('Ctrl Pts',(-1.67996158455503,1.,-0.726235967997433));
#30330=CARTESIAN_POINT('Ctrl Pts',(-1.69326921975743,-1.,-0.731963238697195));
#30331=CARTESIAN_POINT('Ctrl Pts',(-1.69326921975743,1.,-0.731963238697195));
#30332=CARTESIAN_POINT('Ctrl Pts',(-1.70473309006121,-1.,-0.736799665724771));
#30333=CARTESIAN_POINT('Ctrl Pts',(-1.70473309006121,1.,-0.736799665724771));
#30334=CARTESIAN_POINT('Ctrl Pts',(-1.71447789751927,-1.,-0.740795162032087));
#30335=CARTESIAN_POINT('Ctrl Pts',(-1.71447789751927,1.,-0.740795162032087));
#30336=CARTESIAN_POINT('Ctrl Pts',(-1.7226822991693,-1.,-0.744021445433764));
#30337=CARTESIAN_POINT('Ctrl Pts',(-1.7226822991693,1.,-0.744021445433764));
#30338=CARTESIAN_POINT('Ctrl Pts',(-1.72958533647399,-1.,-0.746574710096436));
#30339=CARTESIAN_POINT('Ctrl Pts',(-1.72958533647399,1.,-0.746574710096436));
#30340=CARTESIAN_POINT('Ctrl Pts',(-1.73550351679848,-1.,-0.748582462954854));
#30341=CARTESIAN_POINT('Ctrl Pts',(-1.73550351679848,1.,-0.748582462954854));
#30342=CARTESIAN_POINT('Ctrl Pts',(-1.74080458266705,-1.,-0.75019343597954));
#30343=CARTESIAN_POINT('Ctrl Pts',(-1.74080458266705,1.,-0.75019343597954));
#30344=CARTESIAN_POINT('Ctrl Pts',(-1.74585086852298,-1.,-0.751555614163629));
#30345=CARTESIAN_POINT('Ctrl Pts',(-1.74585086852298,1.,-0.751555614163629));
#30346=CARTESIAN_POINT('Ctrl Pts',(-1.75095139468809,-1.,-0.752797683531377));
#30347=CARTESIAN_POINT('Ctrl Pts',(-1.75095139468809,1.,-0.752797683531377));
#30348=CARTESIAN_POINT('Ctrl Pts',(-1.75631083600175,-1.,-0.75400925402848));
#30349=CARTESIAN_POINT('Ctrl Pts',(-1.75631083600175,1.,-0.75400925402848));
#30350=CARTESIAN_POINT('Ctrl Pts',(-1.7619781724032,-1.,-0.755220979975262));
#30351=CARTESIAN_POINT('Ctrl Pts',(-1.7619781724032,1.,-0.755220979975262));
#30352=CARTESIAN_POINT('Ctrl Pts',(-1.76789396003141,-1.,-0.756421896028403));
#30353=CARTESIAN_POINT('Ctrl Pts',(-1.76789396003141,1.,-0.756421896028403));
#30354=CARTESIAN_POINT('Ctrl Pts',(-1.77394167108342,-1.,-0.757578264077238));
#30355=CARTESIAN_POINT('Ctrl Pts',(-1.77394167108342,1.,-0.757578264077238));
#30356=CARTESIAN_POINT('Ctrl Pts',(-1.77999411220912,-1.,-0.75865062667738));
#30357=CARTESIAN_POINT('Ctrl Pts',(-1.77999411220912,1.,-0.75865062667738));
#30358=CARTESIAN_POINT('Ctrl Pts',(-1.78596964884526,-1.,-0.759614401109868));
#30359=CARTESIAN_POINT('Ctrl Pts',(-1.78596964884526,1.,-0.759614401109868));
#30360=CARTESIAN_POINT('Ctrl Pts',(-1.79185815610802,-1.,-0.760469555880425));
#30361=CARTESIAN_POINT('Ctrl Pts',(-1.79185815610802,1.,-0.760469555880425));
#30362=CARTESIAN_POINT('Ctrl Pts',(-1.79768986997735,-1.,-0.761229695230359));
#30363=CARTESIAN_POINT('Ctrl Pts',(-1.79768986997735,1.,-0.761229695230359));
#30364=CARTESIAN_POINT('Ctrl Pts',(-1.80351583877334,-1.,-0.761915336443515));
#30365=CARTESIAN_POINT('Ctrl Pts',(-1.80351583877334,1.,-0.761915336443515));
#30366=CARTESIAN_POINT('Ctrl Pts',(-1.80938551463989,-1.,-0.762546129464036));
#30367=CARTESIAN_POINT('Ctrl Pts',(-1.80938551463989,1.,-0.762546129464036));
#30368=CARTESIAN_POINT('Ctrl Pts',(-1.81532118405566,-1.,-0.763132003836783));
#30369=CARTESIAN_POINT('Ctrl Pts',(-1.81532118405566,1.,-0.763132003836783));
#30370=CARTESIAN_POINT('Ctrl Pts',(-1.82131873145297,-1.,-0.763673465462854));
#30371=CARTESIAN_POINT('Ctrl Pts',(-1.82131873145297,1.,-0.763673465462854));
#30372=CARTESIAN_POINT('Ctrl Pts',(-1.8273599120008,-1.,-0.764165902606055));
#30373=CARTESIAN_POINT('Ctrl Pts',(-1.8273599120008,1.,-0.764165902606055));
#30374=CARTESIAN_POINT('Ctrl Pts',(-1.8334207722714,-1.,-0.764602549687845));
#30375=CARTESIAN_POINT('Ctrl Pts',(-1.8334207722714,1.,-0.764602549687845));
#30376=CARTESIAN_POINT('Ctrl Pts',(-1.83948181064823,-1.,-0.764978057881687));
#30377=CARTESIAN_POINT('Ctrl Pts',(-1.83948181064823,1.,-0.764978057881687));
#30378=CARTESIAN_POINT('Ctrl Pts',(-1.8455369887591,-1.,-0.765291664861971));
#30379=CARTESIAN_POINT('Ctrl Pts',(-1.8455369887591,1.,-0.765291664861971));
#30380=CARTESIAN_POINT('Ctrl Pts',(-1.85158945130054,-1.,-0.765545710619023));
#30381=CARTESIAN_POINT('Ctrl Pts',(-1.85158945130054,1.,-0.765545710619023));
#30382=CARTESIAN_POINT('Ctrl Pts',(-1.85764741390391,-1.,-0.765744212909305));
#30383=CARTESIAN_POINT('Ctrl Pts',(-1.85764741390391,1.,-0.765744212909305));
#30384=CARTESIAN_POINT('Ctrl Pts',(-1.86372027063314,-1.,-0.765891519092557));
#30385=CARTESIAN_POINT('Ctrl Pts',(-1.86372027063314,1.,-0.765891519092557));
#30386=CARTESIAN_POINT('Ctrl Pts',(-1.86981398314345,-1.,-0.765990708546111));
#30387=CARTESIAN_POINT('Ctrl Pts',(-1.86981398314345,1.,-0.765990708546111));
#30388=CARTESIAN_POINT('Ctrl Pts',(-1.87592888967886,-1.,-0.766042837036759));
#30389=CARTESIAN_POINT('Ctrl Pts',(-1.87592888967886,1.,-0.766042837036759));
#30390=CARTESIAN_POINT('Ctrl Pts',(-1.88206215302561,-1.,-0.766047794851868));
#30391=CARTESIAN_POINT('Ctrl Pts',(-1.88206215302561,1.,-0.766047794851868));
#30392=CARTESIAN_POINT('Ctrl Pts',(-1.88820926433409,-1.,-0.76600483706209));
#30393=CARTESIAN_POINT('Ctrl Pts',(-1.88820926433409,1.,-0.76600483706209));
#30394=CARTESIAN_POINT('Ctrl Pts',(-1.89436577771389,-1.,-0.765913193856979));
#30395=CARTESIAN_POINT('Ctrl Pts',(-1.89436577771389,1.,-0.765913193856979));
#30396=CARTESIAN_POINT('Ctrl Pts',(-1.90052930393599,-1.,-0.765772772593395));
#30397=CARTESIAN_POINT('Ctrl Pts',(-1.90052930393599,1.,-0.765772772593395));
#30398=CARTESIAN_POINT('Ctrl Pts',(-1.90669961402362,-1.,-0.765584196937936));
#30399=CARTESIAN_POINT('Ctrl Pts',(-1.90669961402362,1.,-0.765584196937936));
#30400=CARTESIAN_POINT('Ctrl Pts',(-1.91287765805174,-1.,-0.765348465884739));
#30401=CARTESIAN_POINT('Ctrl Pts',(-1.91287765805174,1.,-0.765348465884739));
#30402=CARTESIAN_POINT('Ctrl Pts',(-1.91906491634197,-1.,-0.765066729667095));
#30403=CARTESIAN_POINT('Ctrl Pts',(-1.91906491634197,1.,-0.765066729667095));
#30404=CARTESIAN_POINT('Ctrl Pts',(-1.92526263537041,-1.,-0.764740025488189));
#30405=CARTESIAN_POINT('Ctrl Pts',(-1.92526263537041,1.,-0.764740025488189));
#30406=CARTESIAN_POINT('Ctrl Pts',(-1.93147105496367,-1.,-0.764369010673889));
#30407=CARTESIAN_POINT('Ctrl Pts',(-1.93147105496367,1.,-0.764369010673889));
#30408=CARTESIAN_POINT('Ctrl Pts',(-1.93768964875867,-1.,-0.763954049121393));
#30409=CARTESIAN_POINT('Ctrl Pts',(-1.93768964875867,1.,-0.763954049121393));
#30410=CARTESIAN_POINT('Ctrl Pts',(-1.94391746617626,-1.,-0.76349533353858));
#30411=CARTESIAN_POINT('Ctrl Pts',(-1.94391746617626,1.,-0.76349533353858));
#30412=CARTESIAN_POINT('Ctrl Pts',(-1.95015342590025,-1.,-0.762992990878774));
#30413=CARTESIAN_POINT('Ctrl Pts',(-1.95015342590025,1.,-0.762992990878774));
#30414=CARTESIAN_POINT('Ctrl Pts',(-1.95639665309893,-1.,-0.762447203806263));
#30415=CARTESIAN_POINT('Ctrl Pts',(-1.95639665309893,1.,-0.762447203806263));
#30416=CARTESIAN_POINT('Ctrl Pts',(-1.96264672744229,-1.,-0.761858300014575));
#30417=CARTESIAN_POINT('Ctrl Pts',(-1.96264672744229,1.,-0.761858300014575));
#30418=CARTESIAN_POINT('Ctrl Pts',(-1.96890351582545,-1.,-0.761226690483986));
#30419=CARTESIAN_POINT('Ctrl Pts',(-1.96890351582545,1.,-0.761226690483986));
#30420=CARTESIAN_POINT('Ctrl Pts',(-1.97516705321521,-1.,-0.760552825409855));
#30421=CARTESIAN_POINT('Ctrl Pts',(-1.97516705321521,1.,-0.760552825409855));
#30422=CARTESIAN_POINT('Ctrl Pts',(-1.98143741418156,-1.,-0.759837147452135));
#30423=CARTESIAN_POINT('Ctrl Pts',(-1.98143741418156,1.,-0.759837147452135));
#30424=CARTESIAN_POINT('Ctrl Pts',(-1.98771456680806,-1.,-0.759080037802242));
#30425=CARTESIAN_POINT('Ctrl Pts',(-1.98771456680806,1.,-0.759080037802242));
#30426=CARTESIAN_POINT('Ctrl Pts',(-1.9939983109871,-1.,-0.758281796766377));
#30427=CARTESIAN_POINT('Ctrl Pts',(-1.9939983109871,1.,-0.758281796766377));
#30428=CARTESIAN_POINT('Ctrl Pts',(-2.00028834739072,-1.,-0.757442676862341));
#30429=CARTESIAN_POINT('Ctrl Pts',(-2.00028834739072,1.,-0.757442676862341));
#30430=CARTESIAN_POINT('Ctrl Pts',(-2.00658431587682,-1.,-0.756562904646496));
#30431=CARTESIAN_POINT('Ctrl Pts',(-2.00658431587682,1.,-0.756562904646496));
#30432=CARTESIAN_POINT('Ctrl Pts',(-2.01288584328149,-1.,-0.7556427049581));
#30433=CARTESIAN_POINT('Ctrl Pts',(-2.01288584328149,1.,-0.7556427049581));
#30434=CARTESIAN_POINT('Ctrl Pts',(-2.01919259406003,-1.,-0.75468233072352));
#30435=CARTESIAN_POINT('Ctrl Pts',(-2.01919259406003,1.,-0.75468233072352));
#30436=CARTESIAN_POINT('Ctrl Pts',(-2.02550428623587,-1.,-0.753682061113765));
#30437=CARTESIAN_POINT('Ctrl Pts',(-2.02550428623587,1.,-0.753682061113765));
#30438=CARTESIAN_POINT('Ctrl Pts',(-2.03182068456467,-1.,-0.752642180488104));
#30439=CARTESIAN_POINT('Ctrl Pts',(-2.03182068456467,1.,-0.752642180488104));
#30440=CARTESIAN_POINT('Ctrl Pts',(-2.03814160092173,-1.,-0.751562963361383));
#30441=CARTESIAN_POINT('Ctrl Pts',(-2.03814160092173,1.,-0.751562963361383));
#30442=CARTESIAN_POINT('Ctrl Pts',(-2.04446689147754,-1.,-0.750444657874758));
#30443=CARTESIAN_POINT('Ctrl Pts',(-2.04446689147754,1.,-0.750444657874758));
#30444=CARTESIAN_POINT('Ctrl Pts',(-2.05079645591606,-1.,-0.749287468663053));
#30445=CARTESIAN_POINT('Ctrl Pts',(-2.05079645591606,1.,-0.749287468663053));
#30446=CARTESIAN_POINT('Ctrl Pts',(-2.05713023030263,-1.,-0.748091554181101));
#30447=CARTESIAN_POINT('Ctrl Pts',(-2.05713023030263,1.,-0.748091554181101));
#30448=CARTESIAN_POINT('Ctrl Pts',(-2.06220058927162,-1.,-0.747103932785504));
#30449=CARTESIAN_POINT('Ctrl Pts',(-2.06220058927162,1.,-0.747103932785504));
#30450=CARTESIAN_POINT('Ctrl Pts',(-2.06600523016401,-1.,-0.746345871542695));
#30451=CARTESIAN_POINT('Ctrl Pts',(-2.06600523016401,1.,-0.746345871542695));
#30452=CARTESIAN_POINT('Ctrl Pts',(-2.06854248895575,-1.,-0.74583279137781));
#30453=CARTESIAN_POINT('Ctrl Pts',(-2.06854248895575,1.,-0.74583279137781));
#30454=CARTESIAN_POINT('Ctrl Pts',(-2.0698113262342,-1.,-0.745574324794401));
#30455=CARTESIAN_POINT('Ctrl Pts',(-2.0698113262342,1.,-0.745574324794401));
#30456=CARTESIAN_POINT('',(-1.60662857109684,1.,-0.693717979106306));
#30457=CARTESIAN_POINT('Ctrl Pts',(-1.60662857109684,1.,-0.693717979106306));
#30458=CARTESIAN_POINT('Ctrl Pts',(-1.61106790958151,1.,-0.695712097881194));
#30459=CARTESIAN_POINT('Ctrl Pts',(-1.61974673472612,1.,-0.699605146405088));
#30460=CARTESIAN_POINT('Ctrl Pts',(-1.63216541664676,1.,-0.705159151988319));
#30461=CARTESIAN_POINT('Ctrl Pts',(-1.64752408832016,1.,-0.711993139355394));
#30462=CARTESIAN_POINT('Ctrl Pts',(-1.6647288055568,1.,-0.719585433804282));
#30463=CARTESIAN_POINT('Ctrl Pts',(-1.67996158455503,1.,-0.726235967997433));
#30464=CARTESIAN_POINT('Ctrl Pts',(-1.69326921975743,1.,-0.731963238697195));
#30465=CARTESIAN_POINT('Ctrl Pts',(-1.70473309006121,1.,-0.736799665724771));
#30466=CARTESIAN_POINT('Ctrl Pts',(-1.71447789751927,1.,-0.740795162032087));
#30467=CARTESIAN_POINT('Ctrl Pts',(-1.7226822991693,1.,-0.744021445433764));
#30468=CARTESIAN_POINT('Ctrl Pts',(-1.72958533647399,1.,-0.746574710096436));
#30469=CARTESIAN_POINT('Ctrl Pts',(-1.73550351679848,1.,-0.748582462954854));
#30470=CARTESIAN_POINT('Ctrl Pts',(-1.74080458266705,1.,-0.75019343597954));
#30471=CARTESIAN_POINT('Ctrl Pts',(-1.74585086852298,1.,-0.751555614163629));
#30472=CARTESIAN_POINT('Ctrl Pts',(-1.75095139468809,1.,-0.752797683531377));
#30473=CARTESIAN_POINT('Ctrl Pts',(-1.75631083600175,1.,-0.75400925402848));
#30474=CARTESIAN_POINT('Ctrl Pts',(-1.7619781724032,1.,-0.755220979975262));
#30475=CARTESIAN_POINT('Ctrl Pts',(-1.76789396003141,1.,-0.756421896028403));
#30476=CARTESIAN_POINT('Ctrl Pts',(-1.77394167108342,1.,-0.757578264077238));
#30477=CARTESIAN_POINT('Ctrl Pts',(-1.77999411220912,1.,-0.75865062667738));
#30478=CARTESIAN_POINT('Ctrl Pts',(-1.78596964884526,1.,-0.759614401109868));
#30479=CARTESIAN_POINT('Ctrl Pts',(-1.79185815610802,1.,-0.760469555880425));
#30480=CARTESIAN_POINT('Ctrl Pts',(-1.79768986997735,1.,-0.761229695230359));
#30481=CARTESIAN_POINT('Ctrl Pts',(-1.80351583877334,1.,-0.761915336443515));
#30482=CARTESIAN_POINT('Ctrl Pts',(-1.80938551463989,1.,-0.762546129464036));
#30483=CARTESIAN_POINT('Ctrl Pts',(-1.81532118405566,1.,-0.763132003836783));
#30484=CARTESIAN_POINT('Ctrl Pts',(-1.82131873145297,1.,-0.763673465462854));
#30485=CARTESIAN_POINT('Ctrl Pts',(-1.8273599120008,1.,-0.764165902606055));
#30486=CARTESIAN_POINT('Ctrl Pts',(-1.8334207722714,1.,-0.764602549687845));
#30487=CARTESIAN_POINT('Ctrl Pts',(-1.83948181064823,1.,-0.764978057881687));
#30488=CARTESIAN_POINT('Ctrl Pts',(-1.8455369887591,1.,-0.765291664861971));
#30489=CARTESIAN_POINT('Ctrl Pts',(-1.85158945130054,1.,-0.765545710619023));
#30490=CARTESIAN_POINT('Ctrl Pts',(-1.85764741390391,1.,-0.765744212909305));
#30491=CARTESIAN_POINT('Ctrl Pts',(-1.86372027063314,1.,-0.765891519092557));
#30492=CARTESIAN_POINT('Ctrl Pts',(-1.86981398314345,1.,-0.765990708546111));
#30493=CARTESIAN_POINT('Ctrl Pts',(-1.87592888967886,1.,-0.766042837036759));
#30494=CARTESIAN_POINT('Ctrl Pts',(-1.88206215302561,1.,-0.766047794851868));
#30495=CARTESIAN_POINT('Ctrl Pts',(-1.88820926433409,1.,-0.76600483706209));
#30496=CARTESIAN_POINT('Ctrl Pts',(-1.89436577771389,1.,-0.765913193856979));
#30497=CARTESIAN_POINT('Ctrl Pts',(-1.90052930393599,1.,-0.765772772593395));
#30498=CARTESIAN_POINT('Ctrl Pts',(-1.90669961402362,1.,-0.765584196937936));
#30499=CARTESIAN_POINT('Ctrl Pts',(-1.91287765805174,1.,-0.765348465884739));
#30500=CARTESIAN_POINT('Ctrl Pts',(-1.91906491634197,1.,-0.765066729667095));
#30501=CARTESIAN_POINT('Ctrl Pts',(-1.92526263537041,1.,-0.764740025488189));
#30502=CARTESIAN_POINT('Ctrl Pts',(-1.93147105496367,1.,-0.764369010673889));
#30503=CARTESIAN_POINT('Ctrl Pts',(-1.93768964875867,1.,-0.763954049121393));
#30504=CARTESIAN_POINT('Ctrl Pts',(-1.94391746617626,1.,-0.76349533353858));
#30505=CARTESIAN_POINT('Ctrl Pts',(-1.95015342590025,1.,-0.762992990878774));
#30506=CARTESIAN_POINT('Ctrl Pts',(-1.95639665309893,1.,-0.762447203806263));
#30507=CARTESIAN_POINT('Ctrl Pts',(-1.96264672744229,1.,-0.761858300014575));
#30508=CARTESIAN_POINT('Ctrl Pts',(-1.96890351582545,1.,-0.761226690483986));
#30509=CARTESIAN_POINT('Ctrl Pts',(-1.97516705321521,1.,-0.760552825409855));
#30510=CARTESIAN_POINT('Ctrl Pts',(-1.98143741418156,1.,-0.759837147452135));
#30511=CARTESIAN_POINT('Ctrl Pts',(-1.98771456680806,1.,-0.759080037802242));
#30512=CARTESIAN_POINT('Ctrl Pts',(-1.9939983109871,1.,-0.758281796766377));
#30513=CARTESIAN_POINT('Ctrl Pts',(-2.00028834739072,1.,-0.757442676862341));
#30514=CARTESIAN_POINT('Ctrl Pts',(-2.00658431587682,1.,-0.756562904646496));
#30515=CARTESIAN_POINT('Ctrl Pts',(-2.01288584328149,1.,-0.7556427049581));
#30516=CARTESIAN_POINT('Ctrl Pts',(-2.01919259406003,1.,-0.75468233072352));
#30517=CARTESIAN_POINT('Ctrl Pts',(-2.02550428623587,1.,-0.753682061113765));
#30518=CARTESIAN_POINT('Ctrl Pts',(-2.03182068456467,1.,-0.752642180488104));
#30519=CARTESIAN_POINT('Ctrl Pts',(-2.03814160092173,1.,-0.751562963361383));
#30520=CARTESIAN_POINT('Ctrl Pts',(-2.04446689147754,1.,-0.750444657874758));
#30521=CARTESIAN_POINT('Ctrl Pts',(-2.05079645591606,1.,-0.749287468663053));
#30522=CARTESIAN_POINT('Ctrl Pts',(-2.05713023030263,1.,-0.748091554181101));
#30523=CARTESIAN_POINT('Ctrl Pts',(-2.06220058927162,1.,-0.747103932785504));
#30524=CARTESIAN_POINT('Ctrl Pts',(-2.06600523016401,1.,-0.746345871542695));
#30525=CARTESIAN_POINT('Ctrl Pts',(-2.06854248895575,1.,-0.74583279137781));
#30526=CARTESIAN_POINT('Ctrl Pts',(-2.0698113262342,1.,-0.745574324794401));
#30527=CARTESIAN_POINT('',(-1.60662857109684,0.,-0.693717979106306));
#30528=CARTESIAN_POINT('Origin',(0.,0.,0.));
#30529=CARTESIAN_POINT('',(-1.5055822144029,1.,-0.892032620296855));
#30530=CARTESIAN_POINT('Origin',(0.,1.,0.));
#30531=CARTESIAN_POINT('',(-1.5055822144029,0.,-0.892032620296855));
#30532=CARTESIAN_POINT('Ctrl Pts',(-1.81978687191668,-1.,-1.23627494547115));
#30533=CARTESIAN_POINT('Ctrl Pts',(-1.81978687191668,1.,-1.23627494547115));
#30534=CARTESIAN_POINT('Ctrl Pts',(-1.81925017193666,-1.,-1.23509651170476));
#30535=CARTESIAN_POINT('Ctrl Pts',(-1.81925017193666,1.,-1.23509651170476));
#30536=CARTESIAN_POINT('Ctrl Pts',(-1.81817389921279,-1.,-1.2327422452705));
#30537=CARTESIAN_POINT('Ctrl Pts',(-1.81817389921279,1.,-1.2327422452705));
#30538=CARTESIAN_POINT('Ctrl Pts',(-1.8165508718364,-1.,-1.2292186489137));
#30539=CARTESIAN_POINT('Ctrl Pts',(-1.8165508718364,1.,-1.2292186489137));
#30540=CARTESIAN_POINT('Ctrl Pts',(-1.81436959210434,-1.,-1.2245361330495));
#30541=CARTESIAN_POINT('Ctrl Pts',(-1.81436959210434,1.,-1.2245361330495));
#30542=CARTESIAN_POINT('Ctrl Pts',(-1.81161420806656,-1.,-1.21870906103557));
#30543=CARTESIAN_POINT('Ctrl Pts',(-1.81161420806656,1.,-1.21870906103557));
#30544=CARTESIAN_POINT('Ctrl Pts',(-1.80882996917129,-1.,-1.21290815708314));
#30545=CARTESIAN_POINT('Ctrl Pts',(-1.80882996917129,1.,-1.21290815708314));
#30546=CARTESIAN_POINT('Ctrl Pts',(-1.80601678480707,-1.,-1.20713356605475));
#30547=CARTESIAN_POINT('Ctrl Pts',(-1.80601678480707,1.,-1.20713356605475));
#30548=CARTESIAN_POINT('Ctrl Pts',(-1.80317454838603,-1.,-1.20138548938974));
#30549=CARTESIAN_POINT('Ctrl Pts',(-1.80317454838603,1.,-1.20138548938974));
#30550=CARTESIAN_POINT('Ctrl Pts',(-1.80030314369879,-1.,-1.19566418930242));
#30551=CARTESIAN_POINT('Ctrl Pts',(-1.80030314369879,1.,-1.19566418930242));
#30552=CARTESIAN_POINT('Ctrl Pts',(-1.79740245923478,-1.,-1.18996997934445));
#30553=CARTESIAN_POINT('Ctrl Pts',(-1.79740245923478,1.,-1.18996997934445));
#30554=CARTESIAN_POINT('Ctrl Pts',(-1.79447240321515,-1.,-1.18430321697432));
#30555=CARTESIAN_POINT('Ctrl Pts',(-1.79447240321515,1.,-1.18430321697432));
#30556=CARTESIAN_POINT('Ctrl Pts',(-1.79151291552689,-1.,-1.17866429440809));
#30557=CARTESIAN_POINT('Ctrl Pts',(-1.79151291552689,1.,-1.17866429440809));
#30558=CARTESIAN_POINT('Ctrl Pts',(-1.78852398877616,-1.,-1.17305363177328));
#30559=CARTESIAN_POINT('Ctrl Pts',(-1.78852398877616,1.,-1.17305363177328));
#30560=CARTESIAN_POINT('Ctrl Pts',(-1.78550566040443,-1.,-1.16747166312303));
#30561=CARTESIAN_POINT('Ctrl Pts',(-1.78550566040443,1.,-1.16747166312303));
#30562=CARTESIAN_POINT('Ctrl Pts',(-1.78245795881009,-1.,-1.16191881298499));
#30563=CARTESIAN_POINT('Ctrl Pts',(-1.78245795881009,1.,-1.16191881298499));
#30564=CARTESIAN_POINT('Ctrl Pts',(-1.77938085564275,-1.,-1.15639547194698));
#30565=CARTESIAN_POINT('Ctrl Pts',(-1.77938085564275,1.,-1.15639547194698));
#30566=CARTESIAN_POINT('Ctrl Pts',(-1.7762742255701,-1.,-1.15090197841515));
#30567=CARTESIAN_POINT('Ctrl Pts',(-1.7762742255701,1.,-1.15090197841515));
#30568=CARTESIAN_POINT('Ctrl Pts',(-1.77313777896194,-1.,-1.1454385822692));
#30569=CARTESIAN_POINT('Ctrl Pts',(-1.77313777896194,1.,-1.1454385822692));
#30570=CARTESIAN_POINT('Ctrl Pts',(-1.76997111386769,-1.,-1.14000548336975));
#30571=CARTESIAN_POINT('Ctrl Pts',(-1.76997111386769,1.,-1.14000548336975));
#30572=CARTESIAN_POINT('Ctrl Pts',(-1.76677384551862,-1.,-1.1346029180462));
#30573=CARTESIAN_POINT('Ctrl Pts',(-1.76677384551862,1.,-1.1346029180462));
#30574=CARTESIAN_POINT('Ctrl Pts',(-1.7635457196617,-1.,-1.12923123555075));
#30575=CARTESIAN_POINT('Ctrl Pts',(-1.7635457196617,1.,-1.12923123555075));
#30576=CARTESIAN_POINT('Ctrl Pts',(-1.76028671825096,-1.,-1.12389096855086));
#30577=CARTESIAN_POINT('Ctrl Pts',(-1.76028671825096,1.,-1.12389096855086));
#30578=CARTESIAN_POINT('Ctrl Pts',(-1.75699720772105,-1.,-1.11858293216763));
#30579=CARTESIAN_POINT('Ctrl Pts',(-1.75699720772105,1.,-1.11858293216763));
#30580=CARTESIAN_POINT('Ctrl Pts',(-1.7536777209463,-1.,-1.11330807582551));
#30581=CARTESIAN_POINT('Ctrl Pts',(-1.7536777209463,1.,-1.11330807582551));
#30582=CARTESIAN_POINT('Ctrl Pts',(-1.7503286607592,-1.,-1.10806728183007));
#30583=CARTESIAN_POINT('Ctrl Pts',(-1.7503286607592,1.,-1.10806728183007));
#30584=CARTESIAN_POINT('Ctrl Pts',(-1.74695004214923,-1.,-1.10286118991143));
#30585=CARTESIAN_POINT('Ctrl Pts',(-1.74695004214923,1.,-1.10286118991143));
#30586=CARTESIAN_POINT('Ctrl Pts',(-1.74354119236208,-1.,-1.09768999241225));
#30587=CARTESIAN_POINT('Ctrl Pts',(-1.74354119236208,1.,-1.09768999241225));
#30588=CARTESIAN_POINT('Ctrl Pts',(-1.74010053962247,-1.,-1.09255329056493));
#30589=CARTESIAN_POINT('Ctrl Pts',(-1.74010053962247,1.,-1.09255329056493));
#30590=CARTESIAN_POINT('Ctrl Pts',(-1.73662628326091,-1.,-1.08745056285427));
#30591=CARTESIAN_POINT('Ctrl Pts',(-1.73662628326091,1.,-1.08745056285427));
#30592=CARTESIAN_POINT('Ctrl Pts',(-1.73311705663407,-1.,-1.08238162784749));
#30593=CARTESIAN_POINT('Ctrl Pts',(-1.73311705663407,1.,-1.08238162784749));
#30594=CARTESIAN_POINT('Ctrl Pts',(-1.72957248977424,-1.,-1.0773470373727));
#30595=CARTESIAN_POINT('Ctrl Pts',(-1.72957248977424,1.,-1.0773470373727));
#30596=CARTESIAN_POINT('Ctrl Pts',(-1.72599406198488,-1.,-1.07234866990252));
#30597=CARTESIAN_POINT('Ctrl Pts',(-1.72599406198488,1.,-1.07234866990252));
#30598=CARTESIAN_POINT('Ctrl Pts',(-1.72238500928453,-1.,-1.06738966975462));
#30599=CARTESIAN_POINT('Ctrl Pts',(-1.72238500928453,1.,-1.06738966975462));
#30600=CARTESIAN_POINT('Ctrl Pts',(-1.71874858456904,-1.,-1.06247324680647));
#30601=CARTESIAN_POINT('Ctrl Pts',(-1.71874858456904,1.,-1.06247324680647));
#30602=CARTESIAN_POINT('Ctrl Pts',(-1.7150865442702,-1.,-1.05760163192479));
#30603=CARTESIAN_POINT('Ctrl Pts',(-1.7150865442702,1.,-1.05760163192479));
#30604=CARTESIAN_POINT('Ctrl Pts',(-1.71139783543989,-1.,-1.05277517202855));
#30605=CARTESIAN_POINT('Ctrl Pts',(-1.71139783543989,1.,-1.05277517202855));
#30606=CARTESIAN_POINT('Ctrl Pts',(-1.70767646263649,-1.,-1.04799085404995));
#30607=CARTESIAN_POINT('Ctrl Pts',(-1.70767646263649,1.,-1.04799085404995));
#30608=CARTESIAN_POINT('Ctrl Pts',(-1.70391338707982,-1.,-1.04324363334554));
#30609=CARTESIAN_POINT('Ctrl Pts',(-1.70391338707982,1.,-1.04324363334554));
#30610=CARTESIAN_POINT('Ctrl Pts',(-1.70010052930962,-1.,-1.03852922490789));
#30611=CARTESIAN_POINT('Ctrl Pts',(-1.70010052930962,1.,-1.03852922490789));
#30612=CARTESIAN_POINT('Ctrl Pts',(-1.69623414782771,-1.,-1.03384646003588));
#30613=CARTESIAN_POINT('Ctrl Pts',(-1.69623414782771,1.,-1.03384646003588));
#30614=CARTESIAN_POINT('Ctrl Pts',(-1.69231840863458,-1.,-1.02919977579147));
#30615=CARTESIAN_POINT('Ctrl Pts',(-1.69231840863458,1.,-1.02919977579147));
#30616=CARTESIAN_POINT('Ctrl Pts',(-1.68836910178447,-1.,-1.02460180535255));
#30617=CARTESIAN_POINT('Ctrl Pts',(-1.68836910178447,1.,-1.02460180535255));
#30618=CARTESIAN_POINT('Ctrl Pts',(-1.68440578021706,-1.,-1.02006795074201));
#30619=CARTESIAN_POINT('Ctrl Pts',(-1.68440578021706,1.,-1.02006795074201));
#30620=CARTESIAN_POINT('Ctrl Pts',(-1.68044289894798,-1.,-1.01561026162773));
#30621=CARTESIAN_POINT('Ctrl Pts',(-1.68044289894798,1.,-1.01561026162773));
#30622=CARTESIAN_POINT('Ctrl Pts',(-1.67648246776464,-1.,-1.01123236493511));
#30623=CARTESIAN_POINT('Ctrl Pts',(-1.67648246776464,1.,-1.01123236493511));
#30624=CARTESIAN_POINT('Ctrl Pts',(-1.67250335383293,-1.,-1.00692206696414));
#30625=CARTESIAN_POINT('Ctrl Pts',(-1.67250335383293,1.,-1.00692206696414));
#30626=CARTESIAN_POINT('Ctrl Pts',(-1.66846059277303,-1.,-1.00265091003727));
#30627=CARTESIAN_POINT('Ctrl Pts',(-1.66846059277303,1.,-1.00265091003727));
#30628=CARTESIAN_POINT('Ctrl Pts',(-1.66430758030376,-1.,-0.998389654952758));
#30629=CARTESIAN_POINT('Ctrl Pts',(-1.66430758030376,1.,-0.998389654952758));
#30630=CARTESIAN_POINT('Ctrl Pts',(-1.66001553809947,-1.,-0.994121836661306));
#30631=CARTESIAN_POINT('Ctrl Pts',(-1.66001553809947,1.,-0.994121836661306));
#30632=CARTESIAN_POINT('Ctrl Pts',(-1.65559044289699,-1.,-0.989855627854165));
#30633=CARTESIAN_POINT('Ctrl Pts',(-1.65559044289699,1.,-0.989855627854165));
#30634=CARTESIAN_POINT('Ctrl Pts',(-1.65110016612638,-1.,-0.985642622920821));
#30635=CARTESIAN_POINT('Ctrl Pts',(-1.65110016612638,1.,-0.985642622920821));
#30636=CARTESIAN_POINT('Ctrl Pts',(-1.64665139190656,-1.,-0.981562530939489));
#30637=CARTESIAN_POINT('Ctrl Pts',(-1.64665139190656,1.,-0.981562530939489));
#30638=CARTESIAN_POINT('Ctrl Pts',(-1.64233990826687,-1.,-0.977689794119416));
#30639=CARTESIAN_POINT('Ctrl Pts',(-1.64233990826687,1.,-0.977689794119416));
#30640=CARTESIAN_POINT('Ctrl Pts',(-1.63820952658144,-1.,-0.974066058287418));
#30641=CARTESIAN_POINT('Ctrl Pts',(-1.63820952658144,1.,-0.974066058287418));
#30642=CARTESIAN_POINT('Ctrl Pts',(-1.63420665729798,-1.,-0.970669715997509));
#30643=CARTESIAN_POINT('Ctrl Pts',(-1.63420665729798,1.,-0.970669715997509));
#30644=CARTESIAN_POINT('Ctrl Pts',(-1.63013849959461,-1.,-0.967387853230345));
#30645=CARTESIAN_POINT('Ctrl Pts',(-1.63013849959461,1.,-0.967387853230345));
#30646=CARTESIAN_POINT('Ctrl Pts',(-1.62571930670187,-1.,-0.964046107040536));
#30647=CARTESIAN_POINT('Ctrl Pts',(-1.62571930670187,1.,-0.964046107040536));
#30648=CARTESIAN_POINT('Ctrl Pts',(-1.62061638140221,-1.,-0.960438326101729));
#30649=CARTESIAN_POINT('Ctrl Pts',(-1.62061638140221,1.,-0.960438326101729));
#30650=CARTESIAN_POINT('Ctrl Pts',(-1.61449324337085,-1.,-0.956354422920671));
#30651=CARTESIAN_POINT('Ctrl Pts',(-1.61449324337085,1.,-0.956354422920671));
#30652=CARTESIAN_POINT('Ctrl Pts',(-1.60706069896936,-1.,-0.951613284356035));
#30653=CARTESIAN_POINT('Ctrl Pts',(-1.60706069896936,1.,-0.951613284356035));
#30654=CARTESIAN_POINT('Ctrl Pts',(-1.59810042043673,-1.,-0.946078063315257));
#30655=CARTESIAN_POINT('Ctrl Pts',(-1.59810042043673,1.,-0.946078063315257));
#30656=CARTESIAN_POINT('Ctrl Pts',(-1.58744937487176,-1.,-0.939646377893399));
#30657=CARTESIAN_POINT('Ctrl Pts',(-1.58744937487176,1.,-0.939646377893399));
#30658=CARTESIAN_POINT('Ctrl Pts',(-1.57499388382243,-1.,-0.932246680108685));
#30659=CARTESIAN_POINT('Ctrl Pts',(-1.57499388382243,1.,-0.932246680108685));
#30660=CARTESIAN_POINT('Ctrl Pts',(-1.56065988578893,-1.,-0.923832188944341));
#30661=CARTESIAN_POINT('Ctrl Pts',(-1.56065988578893,1.,-0.923832188944341));
#30662=CARTESIAN_POINT('Ctrl Pts',(-1.54440491149498,-1.,-0.914375919026456));
#30663=CARTESIAN_POINT('Ctrl Pts',(-1.54440491149498,1.,-0.914375919026456));
#30664=CARTESIAN_POINT('Ctrl Pts',(-1.52984849887993,-1.,-0.905967409625651));
#30665=CARTESIAN_POINT('Ctrl Pts',(-1.52984849887993,1.,-0.905967409625651));
#30666=CARTESIAN_POINT('Ctrl Pts',(-1.51805569590094,-1.,-0.899185047483511));
#30667=CARTESIAN_POINT('Ctrl Pts',(-1.51805569590094,1.,-0.899185047483511));
#30668=CARTESIAN_POINT('Ctrl Pts',(-1.50980486806688,-1.,-0.894452006964543));
#30669=CARTESIAN_POINT('Ctrl Pts',(-1.50980486806688,1.,-0.894452006964543));
#30670=CARTESIAN_POINT('Ctrl Pts',(-1.5055822144029,-1.,-0.892032620296855));
#30671=CARTESIAN_POINT('Ctrl Pts',(-1.5055822144029,1.,-0.892032620296855));
#30672=CARTESIAN_POINT('',(-1.81978687191668,1.,-1.23627494547115));
#30673=CARTESIAN_POINT('Ctrl Pts',(-1.81978687191668,1.,-1.23627494547115));
#30674=CARTESIAN_POINT('Ctrl Pts',(-1.81925017193666,1.,-1.23509651170476));
#30675=CARTESIAN_POINT('Ctrl Pts',(-1.81817389921279,1.,-1.2327422452705));
#30676=CARTESIAN_POINT('Ctrl Pts',(-1.8165508718364,1.,-1.2292186489137));
#30677=CARTESIAN_POINT('Ctrl Pts',(-1.81436959210434,1.,-1.2245361330495));
#30678=CARTESIAN_POINT('Ctrl Pts',(-1.81161420806656,1.,-1.21870906103557));
#30679=CARTESIAN_POINT('Ctrl Pts',(-1.80882996917129,1.,-1.21290815708314));
#30680=CARTESIAN_POINT('Ctrl Pts',(-1.80601678480707,1.,-1.20713356605475));
#30681=CARTESIAN_POINT('Ctrl Pts',(-1.80317454838603,1.,-1.20138548938974));
#30682=CARTESIAN_POINT('Ctrl Pts',(-1.80030314369879,1.,-1.19566418930242));
#30683=CARTESIAN_POINT('Ctrl Pts',(-1.79740245923478,1.,-1.18996997934445));
#30684=CARTESIAN_POINT('Ctrl Pts',(-1.79447240321515,1.,-1.18430321697432));
#30685=CARTESIAN_POINT('Ctrl Pts',(-1.79151291552689,1.,-1.17866429440809));
#30686=CARTESIAN_POINT('Ctrl Pts',(-1.78852398877616,1.,-1.17305363177328));
#30687=CARTESIAN_POINT('Ctrl Pts',(-1.78550566040443,1.,-1.16747166312303));
#30688=CARTESIAN_POINT('Ctrl Pts',(-1.78245795881009,1.,-1.16191881298499));
#30689=CARTESIAN_POINT('Ctrl Pts',(-1.77938085564275,1.,-1.15639547194698));
#30690=CARTESIAN_POINT('Ctrl Pts',(-1.7762742255701,1.,-1.15090197841515));
#30691=CARTESIAN_POINT('Ctrl Pts',(-1.77313777896194,1.,-1.1454385822692));
#30692=CARTESIAN_POINT('Ctrl Pts',(-1.76997111386769,1.,-1.14000548336975));
#30693=CARTESIAN_POINT('Ctrl Pts',(-1.76677384551862,1.,-1.1346029180462));
#30694=CARTESIAN_POINT('Ctrl Pts',(-1.7635457196617,1.,-1.12923123555075));
#30695=CARTESIAN_POINT('Ctrl Pts',(-1.76028671825096,1.,-1.12389096855086));
#30696=CARTESIAN_POINT('Ctrl Pts',(-1.75699720772105,1.,-1.11858293216763));
#30697=CARTESIAN_POINT('Ctrl Pts',(-1.7536777209463,1.,-1.11330807582551));
#30698=CARTESIAN_POINT('Ctrl Pts',(-1.7503286607592,1.,-1.10806728183007));
#30699=CARTESIAN_POINT('Ctrl Pts',(-1.74695004214923,1.,-1.10286118991143));
#30700=CARTESIAN_POINT('Ctrl Pts',(-1.74354119236208,1.,-1.09768999241225));
#30701=CARTESIAN_POINT('Ctrl Pts',(-1.74010053962247,1.,-1.09255329056493));
#30702=CARTESIAN_POINT('Ctrl Pts',(-1.73662628326091,1.,-1.08745056285427));
#30703=CARTESIAN_POINT('Ctrl Pts',(-1.73311705663407,1.,-1.08238162784749));
#30704=CARTESIAN_POINT('Ctrl Pts',(-1.72957248977424,1.,-1.0773470373727));
#30705=CARTESIAN_POINT('Ctrl Pts',(-1.72599406198488,1.,-1.07234866990252));
#30706=CARTESIAN_POINT('Ctrl Pts',(-1.72238500928453,1.,-1.06738966975462));
#30707=CARTESIAN_POINT('Ctrl Pts',(-1.71874858456904,1.,-1.06247324680647));
#30708=CARTESIAN_POINT('Ctrl Pts',(-1.7150865442702,1.,-1.05760163192479));
#30709=CARTESIAN_POINT('Ctrl Pts',(-1.71139783543989,1.,-1.05277517202855));
#30710=CARTESIAN_POINT('Ctrl Pts',(-1.70767646263649,1.,-1.04799085404995));
#30711=CARTESIAN_POINT('Ctrl Pts',(-1.70391338707982,1.,-1.04324363334554));
#30712=CARTESIAN_POINT('Ctrl Pts',(-1.70010052930962,1.,-1.03852922490789));
#30713=CARTESIAN_POINT('Ctrl Pts',(-1.69623414782771,1.,-1.03384646003588));
#30714=CARTESIAN_POINT('Ctrl Pts',(-1.69231840863458,1.,-1.02919977579147));
#30715=CARTESIAN_POINT('Ctrl Pts',(-1.68836910178447,1.,-1.02460180535255));
#30716=CARTESIAN_POINT('Ctrl Pts',(-1.68440578021706,1.,-1.02006795074201));
#30717=CARTESIAN_POINT('Ctrl Pts',(-1.68044289894798,1.,-1.01561026162773));
#30718=CARTESIAN_POINT('Ctrl Pts',(-1.67648246776464,1.,-1.01123236493511));
#30719=CARTESIAN_POINT('Ctrl Pts',(-1.67250335383293,1.,-1.00692206696414));
#30720=CARTESIAN_POINT('Ctrl Pts',(-1.66846059277303,1.,-1.00265091003727));
#30721=CARTESIAN_POINT('Ctrl Pts',(-1.66430758030376,1.,-0.998389654952758));
#30722=CARTESIAN_POINT('Ctrl Pts',(-1.66001553809947,1.,-0.994121836661306));
#30723=CARTESIAN_POINT('Ctrl Pts',(-1.65559044289699,1.,-0.989855627854165));
#30724=CARTESIAN_POINT('Ctrl Pts',(-1.65110016612638,1.,-0.985642622920821));
#30725=CARTESIAN_POINT('Ctrl Pts',(-1.64665139190656,1.,-0.981562530939489));
#30726=CARTESIAN_POINT('Ctrl Pts',(-1.64233990826687,1.,-0.977689794119416));
#30727=CARTESIAN_POINT('Ctrl Pts',(-1.63820952658144,1.,-0.974066058287418));
#30728=CARTESIAN_POINT('Ctrl Pts',(-1.63420665729798,1.,-0.970669715997509));
#30729=CARTESIAN_POINT('Ctrl Pts',(-1.63013849959461,1.,-0.967387853230345));
#30730=CARTESIAN_POINT('Ctrl Pts',(-1.62571930670187,1.,-0.964046107040536));
#30731=CARTESIAN_POINT('Ctrl Pts',(-1.62061638140221,1.,-0.960438326101729));
#30732=CARTESIAN_POINT('Ctrl Pts',(-1.61449324337085,1.,-0.956354422920671));
#30733=CARTESIAN_POINT('Ctrl Pts',(-1.60706069896936,1.,-0.951613284356035));
#30734=CARTESIAN_POINT('Ctrl Pts',(-1.59810042043673,1.,-0.946078063315257));
#30735=CARTESIAN_POINT('Ctrl Pts',(-1.58744937487176,1.,-0.939646377893399));
#30736=CARTESIAN_POINT('Ctrl Pts',(-1.57499388382243,1.,-0.932246680108685));
#30737=CARTESIAN_POINT('Ctrl Pts',(-1.56065988578893,1.,-0.923832188944341));
#30738=CARTESIAN_POINT('Ctrl Pts',(-1.54440491149498,1.,-0.914375919026456));
#30739=CARTESIAN_POINT('Ctrl Pts',(-1.52984849887993,1.,-0.905967409625651));
#30740=CARTESIAN_POINT('Ctrl Pts',(-1.51805569590094,1.,-0.899185047483511));
#30741=CARTESIAN_POINT('Ctrl Pts',(-1.50980486806688,1.,-0.894452006964543));
#30742=CARTESIAN_POINT('Ctrl Pts',(-1.5055822144029,1.,-0.892032620296855));
#30743=CARTESIAN_POINT('',(-1.81978687191668,0.,-1.23627494547115));
#30744=CARTESIAN_POINT('Origin',(-1.73811241238545,0.,-1.34869019493419));
#30745=CARTESIAN_POINT('',(-1.73811241238545,1.,-1.34869019493419));
#30746=CARTESIAN_POINT('',(-1.81978687191668,1.,-1.23627494547115));
#30747=CARTESIAN_POINT('',(-1.73811241238545,0.,-1.34869019493419));
#30748=CARTESIAN_POINT('Ctrl Pts',(-1.31362392696032,-1.,-1.15624053661742));
#30749=CARTESIAN_POINT('Ctrl Pts',(-1.31362392696032,1.,-1.15624053661742));
#30750=CARTESIAN_POINT('Ctrl Pts',(-1.31722977216397,-1.,-1.15950888730809));
#30751=CARTESIAN_POINT('Ctrl Pts',(-1.31722977216397,1.,-1.15950888730809));
#30752=CARTESIAN_POINT('Ctrl Pts',(-1.32428080721772,-1.,-1.16589330093588));
#30753=CARTESIAN_POINT('Ctrl Pts',(-1.32428080721772,1.,-1.16589330093588));
#30754=CARTESIAN_POINT('Ctrl Pts',(-1.33437539347008,-1.,-1.17501305789857));
#30755=CARTESIAN_POINT('Ctrl Pts',(-1.33437539347008,1.,-1.17501305789857));
#30756=CARTESIAN_POINT('Ctrl Pts',(-1.34687054001093,-1.,-1.18625865667441));
#30757=CARTESIAN_POINT('Ctrl Pts',(-1.34687054001093,1.,-1.18625865667441));
#30758=CARTESIAN_POINT('Ctrl Pts',(-1.36088705043885,-1.,-1.1987959077932));
#30759=CARTESIAN_POINT('Ctrl Pts',(-1.36088705043885,1.,-1.1987959077932));
#30760=CARTESIAN_POINT('Ctrl Pts',(-1.37331915607905,-1.,-1.20982812925645));
#30761=CARTESIAN_POINT('Ctrl Pts',(-1.37331915607905,1.,-1.20982812925645));
#30762=CARTESIAN_POINT('Ctrl Pts',(-1.38420564527715,-1.,-1.21938737280852));
#30763=CARTESIAN_POINT('Ctrl Pts',(-1.38420564527715,1.,-1.21938737280852));
#30764=CARTESIAN_POINT('Ctrl Pts',(-1.39361389568796,-1.,-1.22752961899387));
#30765=CARTESIAN_POINT('Ctrl Pts',(-1.39361389568796,1.,-1.22752961899387));
#30766=CARTESIAN_POINT('Ctrl Pts',(-1.40164708206106,-1.,-1.23434087290423));
#30767=CARTESIAN_POINT('Ctrl Pts',(-1.40164708206106,1.,-1.23434087290423));
#30768=CARTESIAN_POINT('Ctrl Pts',(-1.40845295531283,-1.,-1.23994455029534));
#30769=CARTESIAN_POINT('Ctrl Pts',(-1.40845295531283,1.,-1.23994455029534));
#30770=CARTESIAN_POINT('Ctrl Pts',(-1.41422913175179,-1.,-1.24450600513056));
#30771=CARTESIAN_POINT('Ctrl Pts',(-1.41422913175179,1.,-1.24450600513056));
#30772=CARTESIAN_POINT('Ctrl Pts',(-1.41923722596025,-1.,-1.24824430986571));
#30773=CARTESIAN_POINT('Ctrl Pts',(-1.41923722596025,1.,-1.24824430986571));
#30774=CARTESIAN_POINT('Ctrl Pts',(-1.42378102115575,-1.,-1.2514145557001));
#30775=CARTESIAN_POINT('Ctrl Pts',(-1.42378102115575,1.,-1.2514145557001));
#30776=CARTESIAN_POINT('Ctrl Pts',(-1.42815938799387,-1.,-1.25426945222639));
#30777=CARTESIAN_POINT('Ctrl Pts',(-1.42815938799387,1.,-1.25426945222639));
#30778=CARTESIAN_POINT('Ctrl Pts',(-1.43262645609691,-1.,-1.25702687965755));
#30779=CARTESIAN_POINT('Ctrl Pts',(-1.43262645609691,1.,-1.25702687965755));
#30780=CARTESIAN_POINT('Ctrl Pts',(-1.43734919180848,-1.,-1.25983531012005));
#30781=CARTESIAN_POINT('Ctrl Pts',(-1.43734919180848,1.,-1.25983531012005));
#30782=CARTESIAN_POINT('Ctrl Pts',(-1.44236470511303,-1.,-1.26273903323859));
#30783=CARTESIAN_POINT('Ctrl Pts',(-1.44236470511303,1.,-1.26273903323859));
#30784=CARTESIAN_POINT('Ctrl Pts',(-1.44761985001662,-1.,-1.26570925118868));
#30785=CARTESIAN_POINT('Ctrl Pts',(-1.44761985001662,1.,-1.26570925118868));
#30786=CARTESIAN_POINT('Ctrl Pts',(-1.45301422764247,-1.,-1.2686778680489));
#30787=CARTESIAN_POINT('Ctrl Pts',(-1.45301422764247,1.,-1.2686778680489));
#30788=CARTESIAN_POINT('Ctrl Pts',(-1.45843906294697,-1.,-1.27156805265289));
#30789=CARTESIAN_POINT('Ctrl Pts',(-1.45843906294697,1.,-1.27156805265289));
#30790=CARTESIAN_POINT('Ctrl Pts',(-1.46382431332476,-1.,-1.27433119897822));
#30791=CARTESIAN_POINT('Ctrl Pts',(-1.46382431332476,1.,-1.27433119897822));
#30792=CARTESIAN_POINT('Ctrl Pts',(-1.46916035917133,-1.,-1.27696414831089));
#30793=CARTESIAN_POINT('Ctrl Pts',(-1.46916035917133,1.,-1.27696414831089));
#30794=CARTESIAN_POINT('Ctrl Pts',(-1.4744717526707,-1.,-1.2794891824849));
#30795=CARTESIAN_POINT('Ctrl Pts',(-1.4744717526707,1.,-1.2794891824849));
#30796=CARTESIAN_POINT('Ctrl Pts',(-1.47980070347095,-1.,-1.28194158939517));
#30797=CARTESIAN_POINT('Ctrl Pts',(-1.47980070347095,1.,-1.28194158939517));
#30798=CARTESIAN_POINT('Ctrl Pts',(-1.4851881711891,-1.,-1.28435533880201));
#30799=CARTESIAN_POINT('Ctrl Pts',(-1.4851881711891,1.,-1.28435533880201));
#30800=CARTESIAN_POINT('Ctrl Pts',(-1.4906522831278,-1.,-1.2867467611644));
#30801=CARTESIAN_POINT('Ctrl Pts',(-1.4906522831278,1.,-1.2867467611644));
#30802=CARTESIAN_POINT('Ctrl Pts',(-1.49618896881754,-1.,-1.28911506584254));
#30803=CARTESIAN_POINT('Ctrl Pts',(-1.49618896881754,1.,-1.28911506584254));
#30804=CARTESIAN_POINT('Ctrl Pts',(-1.50178230149776,-1.,-1.29145022885181));
#30805=CARTESIAN_POINT('Ctrl Pts',(-1.50178230149776,1.,-1.29145022885181));
#30806=CARTESIAN_POINT('Ctrl Pts',(-1.50741159078365,-1.,-1.29373841372842));
#30807=CARTESIAN_POINT('Ctrl Pts',(-1.50741159078365,1.,-1.29373841372842));
#30808=CARTESIAN_POINT('Ctrl Pts',(-1.51305994241402,-1.,-1.29596850710509));
#30809=CARTESIAN_POINT('Ctrl Pts',(-1.51305994241402,1.,-1.29596850710509));
#30810=CARTESIAN_POINT('Ctrl Pts',(-1.51872184912724,-1.,-1.29813791800747));
#30811=CARTESIAN_POINT('Ctrl Pts',(-1.51872184912724,1.,-1.29813791800747));
#30812=CARTESIAN_POINT('Ctrl Pts',(-1.52439957861062,-1.,-1.30024984366328));
#30813=CARTESIAN_POINT('Ctrl Pts',(-1.52439957861062,1.,-1.30024984366328));
#30814=CARTESIAN_POINT('Ctrl Pts',(-1.53009970283891,-1.,-1.30231064395568));
#30815=CARTESIAN_POINT('Ctrl Pts',(-1.53009970283891,1.,-1.30231064395568));
#30816=CARTESIAN_POINT('Ctrl Pts',(-1.53582981268977,-1.,-1.30432735639489));
#30817=CARTESIAN_POINT('Ctrl Pts',(-1.53582981268977,1.,-1.30432735639489));
#30818=CARTESIAN_POINT('Ctrl Pts',(-1.54159462645432,-1.,-1.30630475189556));
#30819=CARTESIAN_POINT('Ctrl Pts',(-1.54159462645432,1.,-1.30630475189556));
#30820=CARTESIAN_POINT('Ctrl Pts',(-1.54739413957185,-1.,-1.30824393907473));
#30821=CARTESIAN_POINT('Ctrl Pts',(-1.54739413957185,1.,-1.30824393907473));
#30822=CARTESIAN_POINT('Ctrl Pts',(-1.55322568759481,-1.,-1.31014393684222));
#30823=CARTESIAN_POINT('Ctrl Pts',(-1.55322568759481,1.,-1.31014393684222));
#30824=CARTESIAN_POINT('Ctrl Pts',(-1.55908521254821,-1.,-1.31200264341696));
#30825=CARTESIAN_POINT('Ctrl Pts',(-1.55908521254821,1.,-1.31200264341696));
#30826=CARTESIAN_POINT('Ctrl Pts',(-1.56496872402353,-1.,-1.31381795281002));
#30827=CARTESIAN_POINT('Ctrl Pts',(-1.56496872402353,1.,-1.31381795281002));
#30828=CARTESIAN_POINT('Ctrl Pts',(-1.57087397835723,-1.,-1.31558903860016));
#30829=CARTESIAN_POINT('Ctrl Pts',(-1.57087397835723,1.,-1.31558903860016));
#30830=CARTESIAN_POINT('Ctrl Pts',(-1.5768005650559,-1.,-1.31731642317187));
#30831=CARTESIAN_POINT('Ctrl Pts',(-1.5768005650559,1.,-1.31731642317187));
#30832=CARTESIAN_POINT('Ctrl Pts',(-1.58274907898834,-1.,-1.31900135021432));
#30833=CARTESIAN_POINT('Ctrl Pts',(-1.58274907898834,1.,-1.31900135021432));
#30834=CARTESIAN_POINT('Ctrl Pts',(-1.58872057258245,-1.,-1.32064537110892));
#30835=CARTESIAN_POINT('Ctrl Pts',(-1.58872057258245,1.,-1.32064537110892));
#30836=CARTESIAN_POINT('Ctrl Pts',(-1.59471591079403,-1.,-1.32224985747682));
#30837=CARTESIAN_POINT('Ctrl Pts',(-1.59471591079403,1.,-1.32224985747682));
#30838=CARTESIAN_POINT('Ctrl Pts',(-1.60073511858687,-1.,-1.32381550858256));
#30839=CARTESIAN_POINT('Ctrl Pts',(-1.60073511858687,1.,-1.32381550858256));
#30840=CARTESIAN_POINT('Ctrl Pts',(-1.60677758290954,-1.,-1.32534250785782));
#30841=CARTESIAN_POINT('Ctrl Pts',(-1.60677758290954,1.,-1.32534250785782));
#30842=CARTESIAN_POINT('Ctrl Pts',(-1.6128423401575,-1.,-1.32683074483356));
#30843=CARTESIAN_POINT('Ctrl Pts',(-1.6128423401575,1.,-1.32683074483356));
#30844=CARTESIAN_POINT('Ctrl Pts',(-1.61892832270724,-1.,-1.32828000610449));
#30845=CARTESIAN_POINT('Ctrl Pts',(-1.61892832270724,1.,-1.32828000610449));
#30846=CARTESIAN_POINT('Ctrl Pts',(-1.62503464209797,-1.,-1.3296901950568));
#30847=CARTESIAN_POINT('Ctrl Pts',(-1.62503464209797,1.,-1.3296901950568));
#30848=CARTESIAN_POINT('Ctrl Pts',(-1.63116079730923,-1.,-1.33106149345645));
#30849=CARTESIAN_POINT('Ctrl Pts',(-1.63116079730923,1.,-1.33106149345645));
#30850=CARTESIAN_POINT('Ctrl Pts',(-1.63730653475089,-1.,-1.33239425103724));
#30851=CARTESIAN_POINT('Ctrl Pts',(-1.63730653475089,1.,-1.33239425103724));
#30852=CARTESIAN_POINT('Ctrl Pts',(-1.6434717485603,-1.,-1.33368890676572));
#30853=CARTESIAN_POINT('Ctrl Pts',(-1.6434717485603,1.,-1.33368890676572));
#30854=CARTESIAN_POINT('Ctrl Pts',(-1.6496563728683,-1.,-1.33494590467993));
#30855=CARTESIAN_POINT('Ctrl Pts',(-1.6496563728683,1.,-1.33494590467993));
#30856=CARTESIAN_POINT('Ctrl Pts',(-1.65586025952593,-1.,-1.33616559745172));
#30857=CARTESIAN_POINT('Ctrl Pts',(-1.65586025952593,1.,-1.33616559745172));
#30858=CARTESIAN_POINT('Ctrl Pts',(-1.66208312541983,-1.,-1.33734820885262));
#30859=CARTESIAN_POINT('Ctrl Pts',(-1.66208312541983,1.,-1.33734820885262));
#30860=CARTESIAN_POINT('Ctrl Pts',(-1.66832460783989,-1.,-1.33849388654388));
#30861=CARTESIAN_POINT('Ctrl Pts',(-1.66832460783989,1.,-1.33849388654388));
#30862=CARTESIAN_POINT('Ctrl Pts',(-1.67458429426086,-1.,-1.3396027347034));
#30863=CARTESIAN_POINT('Ctrl Pts',(-1.67458429426086,1.,-1.3396027347034));
#30864=CARTESIAN_POINT('Ctrl Pts',(-1.68086176030362,-1.,-1.34067485185203));
#30865=CARTESIAN_POINT('Ctrl Pts',(-1.68086176030362,1.,-1.34067485185203));
#30866=CARTESIAN_POINT('Ctrl Pts',(-1.68715660868764,-1.,-1.341710374848));
#30867=CARTESIAN_POINT('Ctrl Pts',(-1.68715660868764,1.,-1.341710374848));
#30868=CARTESIAN_POINT('Ctrl Pts',(-1.6934684849687,-1.,-1.34270948206319));
#30869=CARTESIAN_POINT('Ctrl Pts',(-1.6934684849687,1.,-1.34270948206319));
#30870=CARTESIAN_POINT('Ctrl Pts',(-1.69979707754427,-1.,-1.34367237124483));
#30871=CARTESIAN_POINT('Ctrl Pts',(-1.69979707754427,1.,-1.34367237124483));
#30872=CARTESIAN_POINT('Ctrl Pts',(-1.70614212266738,-1.,-1.34459924533831));
#30873=CARTESIAN_POINT('Ctrl Pts',(-1.70614212266738,1.,-1.34459924533831));
#30874=CARTESIAN_POINT('Ctrl Pts',(-1.71250340686822,-1.,-1.34549029589416));
#30875=CARTESIAN_POINT('Ctrl Pts',(-1.71250340686822,1.,-1.34549029589416));
#30876=CARTESIAN_POINT('Ctrl Pts',(-1.7188807715049,-1.,-1.34634568653227));
#30877=CARTESIAN_POINT('Ctrl Pts',(-1.7188807715049,1.,-1.34634568653227));
#30878=CARTESIAN_POINT('Ctrl Pts',(-1.72527410680674,-1.,-1.34716554819527));
#30879=CARTESIAN_POINT('Ctrl Pts',(-1.72527410680674,1.,-1.34716554819527));
#30880=CARTESIAN_POINT('Ctrl Pts',(-1.7304014965394,-1.,-1.34779309152035));
#30881=CARTESIAN_POINT('Ctrl Pts',(-1.7304014965394,1.,-1.34779309152035));
#30882=CARTESIAN_POINT('Ctrl Pts',(-1.73425417885907,-1.,-1.34824783112887));
#30883=CARTESIAN_POINT('Ctrl Pts',(-1.73425417885907,1.,-1.34824783112887));
#30884=CARTESIAN_POINT('Ctrl Pts',(-1.73682580585691,-1.,-1.34854391898045));
#30885=CARTESIAN_POINT('Ctrl Pts',(-1.73682580585691,1.,-1.34854391898045));
#30886=CARTESIAN_POINT('Ctrl Pts',(-1.73811241238545,-1.,-1.34869019493419));
#30887=CARTESIAN_POINT('Ctrl Pts',(-1.73811241238545,1.,-1.34869019493419));
#30888=CARTESIAN_POINT('',(-1.31362392696032,1.,-1.15624053661742));
#30889=CARTESIAN_POINT('Ctrl Pts',(-1.31362392696032,1.,-1.15624053661742));
#30890=CARTESIAN_POINT('Ctrl Pts',(-1.31722977216397,1.,-1.15950888730809));
#30891=CARTESIAN_POINT('Ctrl Pts',(-1.32428080721772,1.,-1.16589330093588));
#30892=CARTESIAN_POINT('Ctrl Pts',(-1.33437539347008,1.,-1.17501305789857));
#30893=CARTESIAN_POINT('Ctrl Pts',(-1.34687054001093,1.,-1.18625865667441));
#30894=CARTESIAN_POINT('Ctrl Pts',(-1.36088705043885,1.,-1.1987959077932));
#30895=CARTESIAN_POINT('Ctrl Pts',(-1.37331915607905,1.,-1.20982812925645));
#30896=CARTESIAN_POINT('Ctrl Pts',(-1.38420564527715,1.,-1.21938737280852));
#30897=CARTESIAN_POINT('Ctrl Pts',(-1.39361389568796,1.,-1.22752961899387));
#30898=CARTESIAN_POINT('Ctrl Pts',(-1.40164708206106,1.,-1.23434087290423));
#30899=CARTESIAN_POINT('Ctrl Pts',(-1.40845295531283,1.,-1.23994455029534));
#30900=CARTESIAN_POINT('Ctrl Pts',(-1.41422913175179,1.,-1.24450600513056));
#30901=CARTESIAN_POINT('Ctrl Pts',(-1.41923722596025,1.,-1.24824430986571));
#30902=CARTESIAN_POINT('Ctrl Pts',(-1.42378102115575,1.,-1.2514145557001));
#30903=CARTESIAN_POINT('Ctrl Pts',(-1.42815938799387,1.,-1.25426945222639));
#30904=CARTESIAN_POINT('Ctrl Pts',(-1.43262645609691,1.,-1.25702687965755));
#30905=CARTESIAN_POINT('Ctrl Pts',(-1.43734919180848,1.,-1.25983531012005));
#30906=CARTESIAN_POINT('Ctrl Pts',(-1.44236470511303,1.,-1.26273903323859));
#30907=CARTESIAN_POINT('Ctrl Pts',(-1.44761985001662,1.,-1.26570925118868));
#30908=CARTESIAN_POINT('Ctrl Pts',(-1.45301422764247,1.,-1.2686778680489));
#30909=CARTESIAN_POINT('Ctrl Pts',(-1.45843906294697,1.,-1.27156805265289));
#30910=CARTESIAN_POINT('Ctrl Pts',(-1.46382431332476,1.,-1.27433119897822));
#30911=CARTESIAN_POINT('Ctrl Pts',(-1.46916035917133,1.,-1.27696414831089));
#30912=CARTESIAN_POINT('Ctrl Pts',(-1.4744717526707,1.,-1.2794891824849));
#30913=CARTESIAN_POINT('Ctrl Pts',(-1.47980070347095,1.,-1.28194158939517));
#30914=CARTESIAN_POINT('Ctrl Pts',(-1.4851881711891,1.,-1.28435533880201));
#30915=CARTESIAN_POINT('Ctrl Pts',(-1.4906522831278,1.,-1.2867467611644));
#30916=CARTESIAN_POINT('Ctrl Pts',(-1.49618896881754,1.,-1.28911506584254));
#30917=CARTESIAN_POINT('Ctrl Pts',(-1.50178230149776,1.,-1.29145022885181));
#30918=CARTESIAN_POINT('Ctrl Pts',(-1.50741159078365,1.,-1.29373841372842));
#30919=CARTESIAN_POINT('Ctrl Pts',(-1.51305994241402,1.,-1.29596850710509));
#30920=CARTESIAN_POINT('Ctrl Pts',(-1.51872184912724,1.,-1.29813791800747));
#30921=CARTESIAN_POINT('Ctrl Pts',(-1.52439957861062,1.,-1.30024984366328));
#30922=CARTESIAN_POINT('Ctrl Pts',(-1.53009970283891,1.,-1.30231064395568));
#30923=CARTESIAN_POINT('Ctrl Pts',(-1.53582981268977,1.,-1.30432735639489));
#30924=CARTESIAN_POINT('Ctrl Pts',(-1.54159462645432,1.,-1.30630475189556));
#30925=CARTESIAN_POINT('Ctrl Pts',(-1.54739413957185,1.,-1.30824393907473));
#30926=CARTESIAN_POINT('Ctrl Pts',(-1.55322568759481,1.,-1.31014393684222));
#30927=CARTESIAN_POINT('Ctrl Pts',(-1.55908521254821,1.,-1.31200264341696));
#30928=CARTESIAN_POINT('Ctrl Pts',(-1.56496872402353,1.,-1.31381795281002));
#30929=CARTESIAN_POINT('Ctrl Pts',(-1.57087397835723,1.,-1.31558903860016));
#30930=CARTESIAN_POINT('Ctrl Pts',(-1.5768005650559,1.,-1.31731642317187));
#30931=CARTESIAN_POINT('Ctrl Pts',(-1.58274907898834,1.,-1.31900135021432));
#30932=CARTESIAN_POINT('Ctrl Pts',(-1.58872057258245,1.,-1.32064537110892));
#30933=CARTESIAN_POINT('Ctrl Pts',(-1.59471591079403,1.,-1.32224985747682));
#30934=CARTESIAN_POINT('Ctrl Pts',(-1.60073511858687,1.,-1.32381550858256));
#30935=CARTESIAN_POINT('Ctrl Pts',(-1.60677758290954,1.,-1.32534250785782));
#30936=CARTESIAN_POINT('Ctrl Pts',(-1.6128423401575,1.,-1.32683074483356));
#30937=CARTESIAN_POINT('Ctrl Pts',(-1.61892832270724,1.,-1.32828000610449));
#30938=CARTESIAN_POINT('Ctrl Pts',(-1.62503464209797,1.,-1.3296901950568));
#30939=CARTESIAN_POINT('Ctrl Pts',(-1.63116079730923,1.,-1.33106149345645));
#30940=CARTESIAN_POINT('Ctrl Pts',(-1.63730653475089,1.,-1.33239425103724));
#30941=CARTESIAN_POINT('Ctrl Pts',(-1.6434717485603,1.,-1.33368890676572));
#30942=CARTESIAN_POINT('Ctrl Pts',(-1.6496563728683,1.,-1.33494590467993));
#30943=CARTESIAN_POINT('Ctrl Pts',(-1.65586025952593,1.,-1.33616559745172));
#30944=CARTESIAN_POINT('Ctrl Pts',(-1.66208312541983,1.,-1.33734820885262));
#30945=CARTESIAN_POINT('Ctrl Pts',(-1.66832460783989,1.,-1.33849388654388));
#30946=CARTESIAN_POINT('Ctrl Pts',(-1.67458429426086,1.,-1.3396027347034));
#30947=CARTESIAN_POINT('Ctrl Pts',(-1.68086176030362,1.,-1.34067485185203));
#30948=CARTESIAN_POINT('Ctrl Pts',(-1.68715660868764,1.,-1.341710374848));
#30949=CARTESIAN_POINT('Ctrl Pts',(-1.6934684849687,1.,-1.34270948206319));
#30950=CARTESIAN_POINT('Ctrl Pts',(-1.69979707754427,1.,-1.34367237124483));
#30951=CARTESIAN_POINT('Ctrl Pts',(-1.70614212266738,1.,-1.34459924533831));
#30952=CARTESIAN_POINT('Ctrl Pts',(-1.71250340686822,1.,-1.34549029589416));
#30953=CARTESIAN_POINT('Ctrl Pts',(-1.7188807715049,1.,-1.34634568653227));
#30954=CARTESIAN_POINT('Ctrl Pts',(-1.72527410680674,1.,-1.34716554819527));
#30955=CARTESIAN_POINT('Ctrl Pts',(-1.7304014965394,1.,-1.34779309152035));
#30956=CARTESIAN_POINT('Ctrl Pts',(-1.73425417885907,1.,-1.34824783112887));
#30957=CARTESIAN_POINT('Ctrl Pts',(-1.73682580585691,1.,-1.34854391898045));
#30958=CARTESIAN_POINT('Ctrl Pts',(-1.73811241238545,1.,-1.34869019493419));
#30959=CARTESIAN_POINT('',(-1.31362392696032,0.,-1.15624053661742));
#30960=CARTESIAN_POINT('Origin',(0.,0.,0.));
#30961=CARTESIAN_POINT('',(-1.15624053661742,1.,-1.31362392696033));
#30962=CARTESIAN_POINT('Origin',(0.,1.,0.));
#30963=CARTESIAN_POINT('',(-1.15624053661742,0.,-1.31362392696033));
#30964=CARTESIAN_POINT('Ctrl Pts',(-1.34869019493419,-1.,-1.73811241238545));
#30965=CARTESIAN_POINT('Ctrl Pts',(-1.34869019493419,1.,-1.73811241238545));
#30966=CARTESIAN_POINT('Ctrl Pts',(-1.34854391898145,-1.,-1.73682580585819));
#30967=CARTESIAN_POINT('Ctrl Pts',(-1.34854391898145,1.,-1.73682580585819));
#30968=CARTESIAN_POINT('Ctrl Pts',(-1.34824783113158,-1.,-1.73425417886255));
#30969=CARTESIAN_POINT('Ctrl Pts',(-1.34824783113158,1.,-1.73425417886255));
#30970=CARTESIAN_POINT('Ctrl Pts',(-1.3477930915247,-1.,-1.73040149654497));
#30971=CARTESIAN_POINT('Ctrl Pts',(-1.3477930915247,1.,-1.73040149654497));
#30972=CARTESIAN_POINT('Ctrl Pts',(-1.34716554820013,-1.,-1.72527410681298));
#30973=CARTESIAN_POINT('Ctrl Pts',(-1.34716554820013,1.,-1.72527410681298));
#30974=CARTESIAN_POINT('Ctrl Pts',(-1.34634568653586,-1.,-1.7188807715095));
#30975=CARTESIAN_POINT('Ctrl Pts',(-1.34634568653586,1.,-1.7188807715095));
#30976=CARTESIAN_POINT('Ctrl Pts',(-1.34549029589563,-1.,-1.71250340687011));
#30977=CARTESIAN_POINT('Ctrl Pts',(-1.34549029589563,1.,-1.71250340687011));
#30978=CARTESIAN_POINT('Ctrl Pts',(-1.34459924533783,-1.,-1.70614212266676));
#30979=CARTESIAN_POINT('Ctrl Pts',(-1.34459924533783,1.,-1.70614212266676));
#30980=CARTESIAN_POINT('Ctrl Pts',(-1.34367237124322,-1.,-1.69979707754221));
#30981=CARTESIAN_POINT('Ctrl Pts',(-1.34367237124322,1.,-1.69979707754221));
#30982=CARTESIAN_POINT('Ctrl Pts',(-1.34270948206139,-1.,-1.6934684849664));
#30983=CARTESIAN_POINT('Ctrl Pts',(-1.34270948206139,1.,-1.6934684849664));
#30984=CARTESIAN_POINT('Ctrl Pts',(-1.34171037484673,-1.,-1.68715660868602));
#30985=CARTESIAN_POINT('Ctrl Pts',(-1.34171037484673,1.,-1.68715660868602));
#30986=CARTESIAN_POINT('Ctrl Pts',(-1.3406748518516,-1.,-1.68086176030308));
#30987=CARTESIAN_POINT('Ctrl Pts',(-1.3406748518516,1.,-1.68086176030308));
#30988=CARTESIAN_POINT('Ctrl Pts',(-1.33960273470372,-1.,-1.67458429426126));
#30989=CARTESIAN_POINT('Ctrl Pts',(-1.33960273470372,1.,-1.67458429426126));
#30990=CARTESIAN_POINT('Ctrl Pts',(-1.33849388654458,-1.,-1.66832460784078));
#30991=CARTESIAN_POINT('Ctrl Pts',(-1.33849388654458,1.,-1.66832460784078));
#30992=CARTESIAN_POINT('Ctrl Pts',(-1.33734820885331,-1.,-1.66208312542073));
#30993=CARTESIAN_POINT('Ctrl Pts',(-1.33734820885331,1.,-1.66208312542073));
#30994=CARTESIAN_POINT('Ctrl Pts',(-1.33616559745217,-1.,-1.65586025952651));
#30995=CARTESIAN_POINT('Ctrl Pts',(-1.33616559745217,1.,-1.65586025952651));
#30996=CARTESIAN_POINT('Ctrl Pts',(-1.33494590468003,-1.,-1.64965637286843));
#30997=CARTESIAN_POINT('Ctrl Pts',(-1.33494590468003,1.,-1.64965637286843));
#30998=CARTESIAN_POINT('Ctrl Pts',(-1.33368890676554,-1.,-1.64347174856007));
#30999=CARTESIAN_POINT('Ctrl Pts',(-1.33368890676554,1.,-1.64347174856007));
#31000=CARTESIAN_POINT('Ctrl Pts',(-1.33239425103694,-1.,-1.6373065347505));
#31001=CARTESIAN_POINT('Ctrl Pts',(-1.33239425103694,1.,-1.6373065347505));
#31002=CARTESIAN_POINT('Ctrl Pts',(-1.33106149345618,-1.,-1.63116079730887));
#31003=CARTESIAN_POINT('Ctrl Pts',(-1.33106149345618,1.,-1.63116079730887));
#31004=CARTESIAN_POINT('Ctrl Pts',(-1.32969019505665,-1.,-1.62503464209777));
#31005=CARTESIAN_POINT('Ctrl Pts',(-1.32969019505665,1.,-1.62503464209777));
#31006=CARTESIAN_POINT('Ctrl Pts',(-1.32828000610448,-1.,-1.61892832270723));
#31007=CARTESIAN_POINT('Ctrl Pts',(-1.32828000610448,1.,-1.61892832270723));
#31008=CARTESIAN_POINT('Ctrl Pts',(-1.32683074483365,-1.,-1.61284234015762));
#31009=CARTESIAN_POINT('Ctrl Pts',(-1.32683074483365,1.,-1.61284234015762));
#31010=CARTESIAN_POINT('Ctrl Pts',(-1.32534250785794,-1.,-1.6067775829097));
#31011=CARTESIAN_POINT('Ctrl Pts',(-1.32534250785794,1.,-1.6067775829097));
#31012=CARTESIAN_POINT('Ctrl Pts',(-1.32381550858266,-1.,-1.600735118587));
#31013=CARTESIAN_POINT('Ctrl Pts',(-1.32381550858266,1.,-1.600735118587));
#31014=CARTESIAN_POINT('Ctrl Pts',(-1.32224985747686,-1.,-1.59471591079408));
#31015=CARTESIAN_POINT('Ctrl Pts',(-1.32224985747686,1.,-1.59471591079408));
#31016=CARTESIAN_POINT('Ctrl Pts',(-1.32064537110891,-1.,-1.58872057258244));
#31017=CARTESIAN_POINT('Ctrl Pts',(-1.32064537110891,1.,-1.58872057258244));
#31018=CARTESIAN_POINT('Ctrl Pts',(-1.31900135021428,-1.,-1.58274907898829));
#31019=CARTESIAN_POINT('Ctrl Pts',(-1.31900135021428,1.,-1.58274907898829));
#31020=CARTESIAN_POINT('Ctrl Pts',(-1.31731642317183,-1.,-1.57680056505585));
#31021=CARTESIAN_POINT('Ctrl Pts',(-1.31731642317183,1.,-1.57680056505585));
#31022=CARTESIAN_POINT('Ctrl Pts',(-1.31558903860015,-1.,-1.57087397835721));
#31023=CARTESIAN_POINT('Ctrl Pts',(-1.31558903860015,1.,-1.57087397835721));
#31024=CARTESIAN_POINT('Ctrl Pts',(-1.31381795281002,-1.,-1.56496872402352));
#31025=CARTESIAN_POINT('Ctrl Pts',(-1.31381795281002,1.,-1.56496872402352));
#31026=CARTESIAN_POINT('Ctrl Pts',(-1.31200264341696,-1.,-1.55908521254822));
#31027=CARTESIAN_POINT('Ctrl Pts',(-1.31200264341696,1.,-1.55908521254822));
#31028=CARTESIAN_POINT('Ctrl Pts',(-1.31014393684221,-1.,-1.55322568759481));
#31029=CARTESIAN_POINT('Ctrl Pts',(-1.31014393684221,1.,-1.55322568759481));
#31030=CARTESIAN_POINT('Ctrl Pts',(-1.30824393907471,-1.,-1.54739413957183));
#31031=CARTESIAN_POINT('Ctrl Pts',(-1.30824393907471,1.,-1.54739413957183));
#31032=CARTESIAN_POINT('Ctrl Pts',(-1.30630475189553,-1.,-1.54159462645428));
#31033=CARTESIAN_POINT('Ctrl Pts',(-1.30630475189553,1.,-1.54159462645428));
#31034=CARTESIAN_POINT('Ctrl Pts',(-1.30432735639487,-1.,-1.53582981268976));
#31035=CARTESIAN_POINT('Ctrl Pts',(-1.30432735639487,1.,-1.53582981268976));
#31036=CARTESIAN_POINT('Ctrl Pts',(-1.3023106439557,-1.,-1.53009970283893));
#31037=CARTESIAN_POINT('Ctrl Pts',(-1.3023106439557,1.,-1.53009970283893));
#31038=CARTESIAN_POINT('Ctrl Pts',(-1.30024984366334,-1.,-1.5243995786107));
#31039=CARTESIAN_POINT('Ctrl Pts',(-1.30024984366334,1.,-1.5243995786107));
#31040=CARTESIAN_POINT('Ctrl Pts',(-1.29813791800757,-1.,-1.51872184912735));
#31041=CARTESIAN_POINT('Ctrl Pts',(-1.29813791800757,1.,-1.51872184912735));
#31042=CARTESIAN_POINT('Ctrl Pts',(-1.29596850710518,-1.,-1.51305994241412));
#31043=CARTESIAN_POINT('Ctrl Pts',(-1.29596850710518,1.,-1.51305994241412));
#31044=CARTESIAN_POINT('Ctrl Pts',(-1.29373841372843,-1.,-1.50741159078367));
#31045=CARTESIAN_POINT('Ctrl Pts',(-1.29373841372843,1.,-1.50741159078367));
#31046=CARTESIAN_POINT('Ctrl Pts',(-1.29145022885171,-1.,-1.50178230149764));
#31047=CARTESIAN_POINT('Ctrl Pts',(-1.29145022885171,1.,-1.50178230149764));
#31048=CARTESIAN_POINT('Ctrl Pts',(-1.28911506584232,-1.,-1.49618896881729));
#31049=CARTESIAN_POINT('Ctrl Pts',(-1.28911506584232,1.,-1.49618896881729));
#31050=CARTESIAN_POINT('Ctrl Pts',(-1.28674676116415,-1.,-1.4906522831275));
#31051=CARTESIAN_POINT('Ctrl Pts',(-1.28674676116415,1.,-1.4906522831275));
#31052=CARTESIAN_POINT('Ctrl Pts',(-1.28435533880184,-1.,-1.48518817118891));
#31053=CARTESIAN_POINT('Ctrl Pts',(-1.28435533880184,1.,-1.48518817118891));
#31054=CARTESIAN_POINT('Ctrl Pts',(-1.28194158939522,-1.,-1.47980070347102));
#31055=CARTESIAN_POINT('Ctrl Pts',(-1.28194158939522,1.,-1.47980070347102));
#31056=CARTESIAN_POINT('Ctrl Pts',(-1.27948918248524,-1.,-1.4744717526711));
#31057=CARTESIAN_POINT('Ctrl Pts',(-1.27948918248524,1.,-1.4744717526711));
#31058=CARTESIAN_POINT('Ctrl Pts',(-1.27696414831144,-1.,-1.46916035917197));
#31059=CARTESIAN_POINT('Ctrl Pts',(-1.27696414831144,1.,-1.46916035917197));
#31060=CARTESIAN_POINT('Ctrl Pts',(-1.27433119897877,-1.,-1.4638243133254));
#31061=CARTESIAN_POINT('Ctrl Pts',(-1.27433119897877,1.,-1.4638243133254));
#31062=CARTESIAN_POINT('Ctrl Pts',(-1.27156805265312,-1.,-1.45843906294725));
#31063=CARTESIAN_POINT('Ctrl Pts',(-1.27156805265312,1.,-1.45843906294725));
#31064=CARTESIAN_POINT('Ctrl Pts',(-1.26867786804854,-1.,-1.45301422764205));
#31065=CARTESIAN_POINT('Ctrl Pts',(-1.26867786804854,1.,-1.45301422764205));
#31066=CARTESIAN_POINT('Ctrl Pts',(-1.26570925118767,-1.,-1.44761985001544));
#31067=CARTESIAN_POINT('Ctrl Pts',(-1.26570925118767,1.,-1.44761985001544));
#31068=CARTESIAN_POINT('Ctrl Pts',(-1.26273903323723,-1.,-1.44236470511145));
#31069=CARTESIAN_POINT('Ctrl Pts',(-1.26273903323723,1.,-1.44236470511145));
#31070=CARTESIAN_POINT('Ctrl Pts',(-1.25983531011894,-1.,-1.43734919180719));
#31071=CARTESIAN_POINT('Ctrl Pts',(-1.25983531011894,1.,-1.43734919180719));
#31072=CARTESIAN_POINT('Ctrl Pts',(-1.25702687965744,-1.,-1.43262645609679));
#31073=CARTESIAN_POINT('Ctrl Pts',(-1.25702687965744,1.,-1.43262645609679));
#31074=CARTESIAN_POINT('Ctrl Pts',(-1.25426945222783,-1.,-1.42815938799555));
#31075=CARTESIAN_POINT('Ctrl Pts',(-1.25426945222783,1.,-1.42815938799555));
#31076=CARTESIAN_POINT('Ctrl Pts',(-1.25141455570299,-1.,-1.42378102115911));
#31077=CARTESIAN_POINT('Ctrl Pts',(-1.25141455570299,1.,-1.42378102115911));
#31078=CARTESIAN_POINT('Ctrl Pts',(-1.24824430986911,-1.,-1.41923722596421));
#31079=CARTESIAN_POINT('Ctrl Pts',(-1.24824430986911,1.,-1.41923722596421));
#31080=CARTESIAN_POINT('Ctrl Pts',(-1.24450600513278,-1.,-1.41422913175437));
#31081=CARTESIAN_POINT('Ctrl Pts',(-1.24450600513278,1.,-1.41422913175437));
#31082=CARTESIAN_POINT('Ctrl Pts',(-1.23994455029421,-1.,-1.40845295531151));
#31083=CARTESIAN_POINT('Ctrl Pts',(-1.23994455029421,1.,-1.40845295531151));
#31084=CARTESIAN_POINT('Ctrl Pts',(-1.23434087289768,-1.,-1.40164708205345));
#31085=CARTESIAN_POINT('Ctrl Pts',(-1.23434087289768,1.,-1.40164708205345));
#31086=CARTESIAN_POINT('Ctrl Pts',(-1.22752961898063,-1.,-1.39361389567257));
#31087=CARTESIAN_POINT('Ctrl Pts',(-1.22752961898063,1.,-1.39361389567257));
#31088=CARTESIAN_POINT('Ctrl Pts',(-1.21938737278853,-1.,-1.38420564525391));
#31089=CARTESIAN_POINT('Ctrl Pts',(-1.21938737278853,1.,-1.38420564525391));
#31090=CARTESIAN_POINT('Ctrl Pts',(-1.20982812923113,-1.,-1.37331915604962));
#31091=CARTESIAN_POINT('Ctrl Pts',(-1.20982812923113,1.,-1.37331915604962));
#31092=CARTESIAN_POINT('Ctrl Pts',(-1.1987959077656,-1.,-1.36088705040677));
#31093=CARTESIAN_POINT('Ctrl Pts',(-1.1987959077656,1.,-1.36088705040677));
#31094=CARTESIAN_POINT('Ctrl Pts',(-1.18625865664915,-1.,-1.34687053998157));
#31095=CARTESIAN_POINT('Ctrl Pts',(-1.18625865664915,1.,-1.34687053998157));
#31096=CARTESIAN_POINT('Ctrl Pts',(-1.17501305787994,-1.,-1.33437539344842));
#31097=CARTESIAN_POINT('Ctrl Pts',(-1.17501305787994,1.,-1.33437539344842));
#31098=CARTESIAN_POINT('Ctrl Pts',(-1.16589330092532,-1.,-1.32428080720544));
#31099=CARTESIAN_POINT('Ctrl Pts',(-1.16589330092532,1.,-1.32428080720544));
#31100=CARTESIAN_POINT('Ctrl Pts',(-1.15950888730433,-1.,-1.3172297721596));
#31101=CARTESIAN_POINT('Ctrl Pts',(-1.15950888730433,1.,-1.3172297721596));
#31102=CARTESIAN_POINT('Ctrl Pts',(-1.15624053661742,-1.,-1.31362392696033));
#31103=CARTESIAN_POINT('Ctrl Pts',(-1.15624053661742,1.,-1.31362392696033));
#31104=CARTESIAN_POINT('',(-1.34869019493419,1.,-1.73811241238545));
#31105=CARTESIAN_POINT('Ctrl Pts',(-1.34869019493419,1.,-1.73811241238545));
#31106=CARTESIAN_POINT('Ctrl Pts',(-1.34854391898145,1.,-1.73682580585819));
#31107=CARTESIAN_POINT('Ctrl Pts',(-1.34824783113158,1.,-1.73425417886255));
#31108=CARTESIAN_POINT('Ctrl Pts',(-1.3477930915247,1.,-1.73040149654497));
#31109=CARTESIAN_POINT('Ctrl Pts',(-1.34716554820013,1.,-1.72527410681298));
#31110=CARTESIAN_POINT('Ctrl Pts',(-1.34634568653586,1.,-1.7188807715095));
#31111=CARTESIAN_POINT('Ctrl Pts',(-1.34549029589563,1.,-1.71250340687011));
#31112=CARTESIAN_POINT('Ctrl Pts',(-1.34459924533783,1.,-1.70614212266676));
#31113=CARTESIAN_POINT('Ctrl Pts',(-1.34367237124322,1.,-1.69979707754221));
#31114=CARTESIAN_POINT('Ctrl Pts',(-1.34270948206139,1.,-1.6934684849664));
#31115=CARTESIAN_POINT('Ctrl Pts',(-1.34171037484673,1.,-1.68715660868602));
#31116=CARTESIAN_POINT('Ctrl Pts',(-1.3406748518516,1.,-1.68086176030308));
#31117=CARTESIAN_POINT('Ctrl Pts',(-1.33960273470372,1.,-1.67458429426126));
#31118=CARTESIAN_POINT('Ctrl Pts',(-1.33849388654458,1.,-1.66832460784078));
#31119=CARTESIAN_POINT('Ctrl Pts',(-1.33734820885331,1.,-1.66208312542073));
#31120=CARTESIAN_POINT('Ctrl Pts',(-1.33616559745217,1.,-1.65586025952651));
#31121=CARTESIAN_POINT('Ctrl Pts',(-1.33494590468003,1.,-1.64965637286843));
#31122=CARTESIAN_POINT('Ctrl Pts',(-1.33368890676554,1.,-1.64347174856007));
#31123=CARTESIAN_POINT('Ctrl Pts',(-1.33239425103694,1.,-1.6373065347505));
#31124=CARTESIAN_POINT('Ctrl Pts',(-1.33106149345618,1.,-1.63116079730887));
#31125=CARTESIAN_POINT('Ctrl Pts',(-1.32969019505665,1.,-1.62503464209777));
#31126=CARTESIAN_POINT('Ctrl Pts',(-1.32828000610448,1.,-1.61892832270723));
#31127=CARTESIAN_POINT('Ctrl Pts',(-1.32683074483365,1.,-1.61284234015762));
#31128=CARTESIAN_POINT('Ctrl Pts',(-1.32534250785794,1.,-1.6067775829097));
#31129=CARTESIAN_POINT('Ctrl Pts',(-1.32381550858266,1.,-1.600735118587));
#31130=CARTESIAN_POINT('Ctrl Pts',(-1.32224985747686,1.,-1.59471591079408));
#31131=CARTESIAN_POINT('Ctrl Pts',(-1.32064537110891,1.,-1.58872057258244));
#31132=CARTESIAN_POINT('Ctrl Pts',(-1.31900135021428,1.,-1.58274907898829));
#31133=CARTESIAN_POINT('Ctrl Pts',(-1.31731642317183,1.,-1.57680056505585));
#31134=CARTESIAN_POINT('Ctrl Pts',(-1.31558903860015,1.,-1.57087397835721));
#31135=CARTESIAN_POINT('Ctrl Pts',(-1.31381795281002,1.,-1.56496872402352));
#31136=CARTESIAN_POINT('Ctrl Pts',(-1.31200264341696,1.,-1.55908521254822));
#31137=CARTESIAN_POINT('Ctrl Pts',(-1.31014393684221,1.,-1.55322568759481));
#31138=CARTESIAN_POINT('Ctrl Pts',(-1.30824393907471,1.,-1.54739413957183));
#31139=CARTESIAN_POINT('Ctrl Pts',(-1.30630475189553,1.,-1.54159462645428));
#31140=CARTESIAN_POINT('Ctrl Pts',(-1.30432735639487,1.,-1.53582981268976));
#31141=CARTESIAN_POINT('Ctrl Pts',(-1.3023106439557,1.,-1.53009970283893));
#31142=CARTESIAN_POINT('Ctrl Pts',(-1.30024984366334,1.,-1.5243995786107));
#31143=CARTESIAN_POINT('Ctrl Pts',(-1.29813791800757,1.,-1.51872184912735));
#31144=CARTESIAN_POINT('Ctrl Pts',(-1.29596850710518,1.,-1.51305994241412));
#31145=CARTESIAN_POINT('Ctrl Pts',(-1.29373841372843,1.,-1.50741159078367));
#31146=CARTESIAN_POINT('Ctrl Pts',(-1.29145022885171,1.,-1.50178230149764));
#31147=CARTESIAN_POINT('Ctrl Pts',(-1.28911506584232,1.,-1.49618896881729));
#31148=CARTESIAN_POINT('Ctrl Pts',(-1.28674676116415,1.,-1.4906522831275));
#31149=CARTESIAN_POINT('Ctrl Pts',(-1.28435533880184,1.,-1.48518817118891));
#31150=CARTESIAN_POINT('Ctrl Pts',(-1.28194158939522,1.,-1.47980070347102));
#31151=CARTESIAN_POINT('Ctrl Pts',(-1.27948918248524,1.,-1.4744717526711));
#31152=CARTESIAN_POINT('Ctrl Pts',(-1.27696414831144,1.,-1.46916035917197));
#31153=CARTESIAN_POINT('Ctrl Pts',(-1.27433119897877,1.,-1.4638243133254));
#31154=CARTESIAN_POINT('Ctrl Pts',(-1.27156805265312,1.,-1.45843906294725));
#31155=CARTESIAN_POINT('Ctrl Pts',(-1.26867786804854,1.,-1.45301422764205));
#31156=CARTESIAN_POINT('Ctrl Pts',(-1.26570925118767,1.,-1.44761985001544));
#31157=CARTESIAN_POINT('Ctrl Pts',(-1.26273903323723,1.,-1.44236470511145));
#31158=CARTESIAN_POINT('Ctrl Pts',(-1.25983531011894,1.,-1.43734919180719));
#31159=CARTESIAN_POINT('Ctrl Pts',(-1.25702687965744,1.,-1.43262645609679));
#31160=CARTESIAN_POINT('Ctrl Pts',(-1.25426945222783,1.,-1.42815938799555));
#31161=CARTESIAN_POINT('Ctrl Pts',(-1.25141455570299,1.,-1.42378102115911));
#31162=CARTESIAN_POINT('Ctrl Pts',(-1.24824430986911,1.,-1.41923722596421));
#31163=CARTESIAN_POINT('Ctrl Pts',(-1.24450600513278,1.,-1.41422913175437));
#31164=CARTESIAN_POINT('Ctrl Pts',(-1.23994455029421,1.,-1.40845295531151));
#31165=CARTESIAN_POINT('Ctrl Pts',(-1.23434087289768,1.,-1.40164708205345));
#31166=CARTESIAN_POINT('Ctrl Pts',(-1.22752961898063,1.,-1.39361389567257));
#31167=CARTESIAN_POINT('Ctrl Pts',(-1.21938737278853,1.,-1.38420564525391));
#31168=CARTESIAN_POINT('Ctrl Pts',(-1.20982812923113,1.,-1.37331915604962));
#31169=CARTESIAN_POINT('Ctrl Pts',(-1.1987959077656,1.,-1.36088705040677));
#31170=CARTESIAN_POINT('Ctrl Pts',(-1.18625865664915,1.,-1.34687053998157));
#31171=CARTESIAN_POINT('Ctrl Pts',(-1.17501305787994,1.,-1.33437539344842));
#31172=CARTESIAN_POINT('Ctrl Pts',(-1.16589330092532,1.,-1.32428080720544));
#31173=CARTESIAN_POINT('Ctrl Pts',(-1.15950888730433,1.,-1.3172297721596));
#31174=CARTESIAN_POINT('Ctrl Pts',(-1.15624053661742,1.,-1.31362392696033));
#31175=CARTESIAN_POINT('',(-1.34869019493419,0.,-1.73811241238545));
#31176=CARTESIAN_POINT('Origin',(-1.23627494547115,0.,-1.81978687191668));
#31177=CARTESIAN_POINT('',(-1.23627494547115,1.,-1.81978687191668));
#31178=CARTESIAN_POINT('',(-1.34869019493419,1.,-1.73811241238545));
#31179=CARTESIAN_POINT('',(-1.23627494547115,0.,-1.81978687191668));
#31180=CARTESIAN_POINT('Ctrl Pts',(-0.892032620296855,-1.,-1.5055822144029));
#31181=CARTESIAN_POINT('Ctrl Pts',(-0.892032620296855,1.,-1.5055822144029));
#31182=CARTESIAN_POINT('Ctrl Pts',(-0.894452006967538,-1.,-1.50980486807181));
#31183=CARTESIAN_POINT('Ctrl Pts',(-0.894452006967538,1.,-1.50980486807181));
#31184=CARTESIAN_POINT('Ctrl Pts',(-0.89918504749193,-1.,-1.51805569591479));
#31185=CARTESIAN_POINT('Ctrl Pts',(-0.89918504749193,1.,-1.51805569591479));
#31186=CARTESIAN_POINT('Ctrl Pts',(-0.905967409640499,-1.,-1.52984849890434));
#31187=CARTESIAN_POINT('Ctrl Pts',(-0.905967409640499,1.,-1.52984849890434));
#31188=CARTESIAN_POINT('Ctrl Pts',(-0.91437591904658,-1.,-1.54440491152808));
#31189=CARTESIAN_POINT('Ctrl Pts',(-0.91437591904658,1.,-1.54440491152808));
#31190=CARTESIAN_POINT('Ctrl Pts',(-0.923832188966322,-1.,-1.56065988582509));
#31191=CARTESIAN_POINT('Ctrl Pts',(-0.923832188966322,1.,-1.56065988582509));
#31192=CARTESIAN_POINT('Ctrl Pts',(-0.932246680128849,-1.,-1.57499388385561));
#31193=CARTESIAN_POINT('Ctrl Pts',(-0.932246680128849,1.,-1.57499388385561));
#31194=CARTESIAN_POINT('Ctrl Pts',(-0.939646377909319,-1.,-1.58744937489796));
#31195=CARTESIAN_POINT('Ctrl Pts',(-0.939646377909319,1.,-1.58744937489796));
#31196=CARTESIAN_POINT('Ctrl Pts',(-0.946078063325796,-1.,-1.59810042045408));
#31197=CARTESIAN_POINT('Ctrl Pts',(-0.946078063325796,1.,-1.59810042045408));
#31198=CARTESIAN_POINT('Ctrl Pts',(-0.951613284361248,-1.,-1.60706069897794));
#31199=CARTESIAN_POINT('Ctrl Pts',(-0.951613284361248,1.,-1.60706069897794));
#31200=CARTESIAN_POINT('Ctrl Pts',(-0.956354422921573,-1.,-1.61449324337233));
#31201=CARTESIAN_POINT('Ctrl Pts',(-0.956354422921573,1.,-1.61449324337233));
#31202=CARTESIAN_POINT('Ctrl Pts',(-0.960438326099958,-1.,-1.62061638139929));
#31203=CARTESIAN_POINT('Ctrl Pts',(-0.960438326099958,1.,-1.62061638139929));
#31204=CARTESIAN_POINT('Ctrl Pts',(-0.964046107037821,-1.,-1.6257193066974));
#31205=CARTESIAN_POINT('Ctrl Pts',(-0.964046107037821,1.,-1.6257193066974));
#31206=CARTESIAN_POINT('Ctrl Pts',(-0.967387853228041,-1.,-1.63013849959083));
#31207=CARTESIAN_POINT('Ctrl Pts',(-0.967387853228041,1.,-1.63013849959083));
#31208=CARTESIAN_POINT('Ctrl Pts',(-0.970669715996356,-1.,-1.63420665729609));
#31209=CARTESIAN_POINT('Ctrl Pts',(-0.970669715996356,1.,-1.63420665729609));
#31210=CARTESIAN_POINT('Ctrl Pts',(-0.974066058287501,-1.,-1.63820952658157));
#31211=CARTESIAN_POINT('Ctrl Pts',(-0.974066058287501,1.,-1.63820952658157));
#31212=CARTESIAN_POINT('Ctrl Pts',(-0.977689794120297,-1.,-1.64233990826831));
#31213=CARTESIAN_POINT('Ctrl Pts',(-0.977689794120297,1.,-1.64233990826831));
#31214=CARTESIAN_POINT('Ctrl Pts',(-0.981562530940574,-1.,-1.64665139190834));
#31215=CARTESIAN_POINT('Ctrl Pts',(-0.981562530940574,1.,-1.64665139190834));
#31216=CARTESIAN_POINT('Ctrl Pts',(-0.985642622921626,-1.,-1.6511001661277));
#31217=CARTESIAN_POINT('Ctrl Pts',(-0.985642622921626,1.,-1.6511001661277));
#31218=CARTESIAN_POINT('Ctrl Pts',(-0.98985562785445,-1.,-1.65559044289746));
#31219=CARTESIAN_POINT('Ctrl Pts',(-0.98985562785445,1.,-1.65559044289746));
#31220=CARTESIAN_POINT('Ctrl Pts',(-0.994121836661116,-1.,-1.66001553809916));
#31221=CARTESIAN_POINT('Ctrl Pts',(-0.994121836661116,1.,-1.66001553809916));
#31222=CARTESIAN_POINT('Ctrl Pts',(-0.998389654952317,-1.,-1.66430758030304));
#31223=CARTESIAN_POINT('Ctrl Pts',(-0.998389654952317,1.,-1.66430758030304));
#31224=CARTESIAN_POINT('Ctrl Pts',(-1.00265091003682,-1.,-1.66846059277231));
#31225=CARTESIAN_POINT('Ctrl Pts',(-1.00265091003682,1.,-1.66846059277231));
#31226=CARTESIAN_POINT('Ctrl Pts',(-1.00692206696387,-1.,-1.67250335383248));
#31227=CARTESIAN_POINT('Ctrl Pts',(-1.00692206696387,1.,-1.67250335383248));
#31228=CARTESIAN_POINT('Ctrl Pts',(-1.01123236493507,-1.,-1.67648246776457));
#31229=CARTESIAN_POINT('Ctrl Pts',(-1.01123236493507,1.,-1.67648246776457));
#31230=CARTESIAN_POINT('Ctrl Pts',(-1.01561026162787,-1.,-1.6804428989482));
#31231=CARTESIAN_POINT('Ctrl Pts',(-1.01561026162787,1.,-1.6804428989482));
#31232=CARTESIAN_POINT('Ctrl Pts',(-1.02006795074222,-1.,-1.68440578021739));
#31233=CARTESIAN_POINT('Ctrl Pts',(-1.02006795074222,1.,-1.68440578021739));
#31234=CARTESIAN_POINT('Ctrl Pts',(-1.02460180535272,-1.,-1.68836910178475));
#31235=CARTESIAN_POINT('Ctrl Pts',(-1.02460180535272,1.,-1.68836910178475));
#31236=CARTESIAN_POINT('Ctrl Pts',(-1.02919977579155,-1.,-1.69231840863471));
#31237=CARTESIAN_POINT('Ctrl Pts',(-1.02919977579155,1.,-1.69231840863471));
#31238=CARTESIAN_POINT('Ctrl Pts',(-1.03384646003587,-1.,-1.69623414782769));
#31239=CARTESIAN_POINT('Ctrl Pts',(-1.03384646003587,1.,-1.69623414782769));
#31240=CARTESIAN_POINT('Ctrl Pts',(-1.03852922490782,-1.,-1.70010052930951));
#31241=CARTESIAN_POINT('Ctrl Pts',(-1.03852922490782,1.,-1.70010052930951));
#31242=CARTESIAN_POINT('Ctrl Pts',(-1.04324363334546,-1.,-1.70391338707969));
#31243=CARTESIAN_POINT('Ctrl Pts',(-1.04324363334546,1.,-1.70391338707969));
#31244=CARTESIAN_POINT('Ctrl Pts',(-1.0479908540499,-1.,-1.70767646263641));
#31245=CARTESIAN_POINT('Ctrl Pts',(-1.0479908540499,1.,-1.70767646263641));
#31246=CARTESIAN_POINT('Ctrl Pts',(-1.05277517202854,-1.,-1.71139783543986));
#31247=CARTESIAN_POINT('Ctrl Pts',(-1.05277517202854,1.,-1.71139783543986));
#31248=CARTESIAN_POINT('Ctrl Pts',(-1.05760163192481,-1.,-1.71508654427022));
#31249=CARTESIAN_POINT('Ctrl Pts',(-1.05760163192481,1.,-1.71508654427022));
#31250=CARTESIAN_POINT('Ctrl Pts',(-1.0624732468065,-1.,-1.71874858456908));
#31251=CARTESIAN_POINT('Ctrl Pts',(-1.0624732468065,1.,-1.71874858456908));
#31252=CARTESIAN_POINT('Ctrl Pts',(-1.06738966975463,-1.,-1.72238500928456));
#31253=CARTESIAN_POINT('Ctrl Pts',(-1.06738966975463,1.,-1.72238500928456));
#31254=CARTESIAN_POINT('Ctrl Pts',(-1.07234866990252,-1.,-1.72599406198489));
#31255=CARTESIAN_POINT('Ctrl Pts',(-1.07234866990252,1.,-1.72599406198489));
#31256=CARTESIAN_POINT('Ctrl Pts',(-1.0773470373727,-1.,-1.72957248977424));
#31257=CARTESIAN_POINT('Ctrl Pts',(-1.0773470373727,1.,-1.72957248977424));
#31258=CARTESIAN_POINT('Ctrl Pts',(-1.08238162784749,-1.,-1.73311705663407));
#31259=CARTESIAN_POINT('Ctrl Pts',(-1.08238162784749,1.,-1.73311705663407));
#31260=CARTESIAN_POINT('Ctrl Pts',(-1.08745056285429,-1.,-1.73662628326093));
#31261=CARTESIAN_POINT('Ctrl Pts',(-1.08745056285429,1.,-1.73662628326093));
#31262=CARTESIAN_POINT('Ctrl Pts',(-1.09255329056496,-1.,-1.74010053962252));
#31263=CARTESIAN_POINT('Ctrl Pts',(-1.09255329056496,1.,-1.74010053962252));
#31264=CARTESIAN_POINT('Ctrl Pts',(-1.09768999241229,-1.,-1.74354119236212));
#31265=CARTESIAN_POINT('Ctrl Pts',(-1.09768999241229,1.,-1.74354119236212));
#31266=CARTESIAN_POINT('Ctrl Pts',(-1.10286118991144,-1.,-1.74695004214924));
#31267=CARTESIAN_POINT('Ctrl Pts',(-1.10286118991144,1.,-1.74695004214924));
#31268=CARTESIAN_POINT('Ctrl Pts',(-1.10806728183003,-1.,-1.75032866075914));
#31269=CARTESIAN_POINT('Ctrl Pts',(-1.10806728183003,1.,-1.75032866075914));
#31270=CARTESIAN_POINT('Ctrl Pts',(-1.11330807582542,-1.,-1.75367772094617));
#31271=CARTESIAN_POINT('Ctrl Pts',(-1.11330807582542,1.,-1.75367772094617));
#31272=CARTESIAN_POINT('Ctrl Pts',(-1.11858293216752,-1.,-1.75699720772089));
#31273=CARTESIAN_POINT('Ctrl Pts',(-1.11858293216752,1.,-1.75699720772089));
#31274=CARTESIAN_POINT('Ctrl Pts',(-1.12389096855078,-1.,-1.76028671825084));
#31275=CARTESIAN_POINT('Ctrl Pts',(-1.12389096855078,1.,-1.76028671825084));
#31276=CARTESIAN_POINT('Ctrl Pts',(-1.12923123555076,-1.,-1.76354571966171));
#31277=CARTESIAN_POINT('Ctrl Pts',(-1.12923123555076,1.,-1.76354571966171));
#31278=CARTESIAN_POINT('Ctrl Pts',(-1.13460291804635,-1.,-1.76677384551883));
#31279=CARTESIAN_POINT('Ctrl Pts',(-1.13460291804635,1.,-1.76677384551883));
#31280=CARTESIAN_POINT('Ctrl Pts',(-1.14000548337,-1.,-1.76997111386806));
#31281=CARTESIAN_POINT('Ctrl Pts',(-1.14000548337,1.,-1.76997111386806));
#31282=CARTESIAN_POINT('Ctrl Pts',(-1.14543858226948,-1.,-1.77313777896234));
#31283=CARTESIAN_POINT('Ctrl Pts',(-1.14543858226948,1.,-1.77313777896234));
#31284=CARTESIAN_POINT('Ctrl Pts',(-1.15090197841531,-1.,-1.77627422557034));
#31285=CARTESIAN_POINT('Ctrl Pts',(-1.15090197841531,1.,-1.77627422557034));
#31286=CARTESIAN_POINT('Ctrl Pts',(-1.15639547194689,-1.,-1.77938085564261));
#31287=CARTESIAN_POINT('Ctrl Pts',(-1.15639547194689,1.,-1.77938085564261));
#31288=CARTESIAN_POINT('Ctrl Pts',(-1.16191881298458,-1.,-1.78245795880949));
#31289=CARTESIAN_POINT('Ctrl Pts',(-1.16191881298458,1.,-1.78245795880949));
#31290=CARTESIAN_POINT('Ctrl Pts',(-1.16747166312239,-1.,-1.78550566040349));
#31291=CARTESIAN_POINT('Ctrl Pts',(-1.16747166312239,1.,-1.78550566040349));
#31292=CARTESIAN_POINT('Ctrl Pts',(-1.17305363177265,-1.,-1.78852398877523));
#31293=CARTESIAN_POINT('Ctrl Pts',(-1.17305363177265,1.,-1.78852398877523));
#31294=CARTESIAN_POINT('Ctrl Pts',(-1.17866429440781,-1.,-1.79151291552646));
#31295=CARTESIAN_POINT('Ctrl Pts',(-1.17866429440781,1.,-1.79151291552646));
#31296=CARTESIAN_POINT('Ctrl Pts',(-1.18430321697471,-1.,-1.79447240321572));
#31297=CARTESIAN_POINT('Ctrl Pts',(-1.18430321697471,1.,-1.79447240321572));
#31298=CARTESIAN_POINT('Ctrl Pts',(-1.1899699793456,-1.,-1.79740245923649));
#31299=CARTESIAN_POINT('Ctrl Pts',(-1.1899699793456,1.,-1.79740245923649));
#31300=CARTESIAN_POINT('Ctrl Pts',(-1.19566418930405,-1.,-1.80030314370121));
#31301=CARTESIAN_POINT('Ctrl Pts',(-1.19566418930405,1.,-1.80030314370121));
#31302=CARTESIAN_POINT('Ctrl Pts',(-1.2013854893912,-1.,-1.8031745483882));
#31303=CARTESIAN_POINT('Ctrl Pts',(-1.2013854893912,1.,-1.8031745483882));
#31304=CARTESIAN_POINT('Ctrl Pts',(-1.20713356605519,-1.,-1.80601678480772));
#31305=CARTESIAN_POINT('Ctrl Pts',(-1.20713356605519,1.,-1.80601678480772));
#31306=CARTESIAN_POINT('Ctrl Pts',(-1.2129081570818,-1.,-1.80882996916931));
#31307=CARTESIAN_POINT('Ctrl Pts',(-1.2129081570818,1.,-1.80882996916931));
#31308=CARTESIAN_POINT('Ctrl Pts',(-1.2187090610323,-1.,-1.81161420806172));
#31309=CARTESIAN_POINT('Ctrl Pts',(-1.2187090610323,1.,-1.81161420806172));
#31310=CARTESIAN_POINT('Ctrl Pts',(-1.22453613304507,-1.,-1.81436959209778));
#31311=CARTESIAN_POINT('Ctrl Pts',(-1.22453613304507,1.,-1.81436959209778));
#31312=CARTESIAN_POINT('Ctrl Pts',(-1.22921864890975,-1.,-1.81655087183054));
#31313=CARTESIAN_POINT('Ctrl Pts',(-1.22921864890975,1.,-1.81655087183054));
#31314=CARTESIAN_POINT('Ctrl Pts',(-1.23274224526804,-1.,-1.81817389920914));
#31315=CARTESIAN_POINT('Ctrl Pts',(-1.23274224526804,1.,-1.81817389920914));
#31316=CARTESIAN_POINT('Ctrl Pts',(-1.23509651170384,-1.,-1.81925017193531));
#31317=CARTESIAN_POINT('Ctrl Pts',(-1.23509651170384,1.,-1.81925017193531));
#31318=CARTESIAN_POINT('Ctrl Pts',(-1.23627494547115,-1.,-1.81978687191668));
#31319=CARTESIAN_POINT('Ctrl Pts',(-1.23627494547115,1.,-1.81978687191668));
#31320=CARTESIAN_POINT('',(-0.892032620296855,1.,-1.5055822144029));
#31321=CARTESIAN_POINT('Ctrl Pts',(-0.892032620296855,1.,-1.5055822144029));
#31322=CARTESIAN_POINT('Ctrl Pts',(-0.894452006967538,1.,-1.50980486807181));
#31323=CARTESIAN_POINT('Ctrl Pts',(-0.89918504749193,1.,-1.51805569591479));
#31324=CARTESIAN_POINT('Ctrl Pts',(-0.905967409640499,1.,-1.52984849890434));
#31325=CARTESIAN_POINT('Ctrl Pts',(-0.91437591904658,1.,-1.54440491152808));
#31326=CARTESIAN_POINT('Ctrl Pts',(-0.923832188966322,1.,-1.56065988582509));
#31327=CARTESIAN_POINT('Ctrl Pts',(-0.932246680128849,1.,-1.57499388385561));
#31328=CARTESIAN_POINT('Ctrl Pts',(-0.939646377909319,1.,-1.58744937489796));
#31329=CARTESIAN_POINT('Ctrl Pts',(-0.946078063325796,1.,-1.59810042045408));
#31330=CARTESIAN_POINT('Ctrl Pts',(-0.951613284361248,1.,-1.60706069897794));
#31331=CARTESIAN_POINT('Ctrl Pts',(-0.956354422921573,1.,-1.61449324337233));
#31332=CARTESIAN_POINT('Ctrl Pts',(-0.960438326099958,1.,-1.62061638139929));
#31333=CARTESIAN_POINT('Ctrl Pts',(-0.964046107037821,1.,-1.6257193066974));
#31334=CARTESIAN_POINT('Ctrl Pts',(-0.967387853228041,1.,-1.63013849959083));
#31335=CARTESIAN_POINT('Ctrl Pts',(-0.970669715996356,1.,-1.63420665729609));
#31336=CARTESIAN_POINT('Ctrl Pts',(-0.974066058287501,1.,-1.63820952658157));
#31337=CARTESIAN_POINT('Ctrl Pts',(-0.977689794120297,1.,-1.64233990826831));
#31338=CARTESIAN_POINT('Ctrl Pts',(-0.981562530940574,1.,-1.64665139190834));
#31339=CARTESIAN_POINT('Ctrl Pts',(-0.985642622921626,1.,-1.6511001661277));
#31340=CARTESIAN_POINT('Ctrl Pts',(-0.98985562785445,1.,-1.65559044289746));
#31341=CARTESIAN_POINT('Ctrl Pts',(-0.994121836661116,1.,-1.66001553809916));
#31342=CARTESIAN_POINT('Ctrl Pts',(-0.998389654952317,1.,-1.66430758030304));
#31343=CARTESIAN_POINT('Ctrl Pts',(-1.00265091003682,1.,-1.66846059277231));
#31344=CARTESIAN_POINT('Ctrl Pts',(-1.00692206696387,1.,-1.67250335383248));
#31345=CARTESIAN_POINT('Ctrl Pts',(-1.01123236493507,1.,-1.67648246776457));
#31346=CARTESIAN_POINT('Ctrl Pts',(-1.01561026162787,1.,-1.6804428989482));
#31347=CARTESIAN_POINT('Ctrl Pts',(-1.02006795074222,1.,-1.68440578021739));
#31348=CARTESIAN_POINT('Ctrl Pts',(-1.02460180535272,1.,-1.68836910178475));
#31349=CARTESIAN_POINT('Ctrl Pts',(-1.02919977579155,1.,-1.69231840863471));
#31350=CARTESIAN_POINT('Ctrl Pts',(-1.03384646003587,1.,-1.69623414782769));
#31351=CARTESIAN_POINT('Ctrl Pts',(-1.03852922490782,1.,-1.70010052930951));
#31352=CARTESIAN_POINT('Ctrl Pts',(-1.04324363334546,1.,-1.70391338707969));
#31353=CARTESIAN_POINT('Ctrl Pts',(-1.0479908540499,1.,-1.70767646263641));
#31354=CARTESIAN_POINT('Ctrl Pts',(-1.05277517202854,1.,-1.71139783543986));
#31355=CARTESIAN_POINT('Ctrl Pts',(-1.05760163192481,1.,-1.71508654427022));
#31356=CARTESIAN_POINT('Ctrl Pts',(-1.0624732468065,1.,-1.71874858456908));
#31357=CARTESIAN_POINT('Ctrl Pts',(-1.06738966975463,1.,-1.72238500928456));
#31358=CARTESIAN_POINT('Ctrl Pts',(-1.07234866990252,1.,-1.72599406198489));
#31359=CARTESIAN_POINT('Ctrl Pts',(-1.0773470373727,1.,-1.72957248977424));
#31360=CARTESIAN_POINT('Ctrl Pts',(-1.08238162784749,1.,-1.73311705663407));
#31361=CARTESIAN_POINT('Ctrl Pts',(-1.08745056285429,1.,-1.73662628326093));
#31362=CARTESIAN_POINT('Ctrl Pts',(-1.09255329056496,1.,-1.74010053962252));
#31363=CARTESIAN_POINT('Ctrl Pts',(-1.09768999241229,1.,-1.74354119236212));
#31364=CARTESIAN_POINT('Ctrl Pts',(-1.10286118991144,1.,-1.74695004214924));
#31365=CARTESIAN_POINT('Ctrl Pts',(-1.10806728183003,1.,-1.75032866075914));
#31366=CARTESIAN_POINT('Ctrl Pts',(-1.11330807582542,1.,-1.75367772094617));
#31367=CARTESIAN_POINT('Ctrl Pts',(-1.11858293216752,1.,-1.75699720772089));
#31368=CARTESIAN_POINT('Ctrl Pts',(-1.12389096855078,1.,-1.76028671825084));
#31369=CARTESIAN_POINT('Ctrl Pts',(-1.12923123555076,1.,-1.76354571966171));
#31370=CARTESIAN_POINT('Ctrl Pts',(-1.13460291804635,1.,-1.76677384551883));
#31371=CARTESIAN_POINT('Ctrl Pts',(-1.14000548337,1.,-1.76997111386806));
#31372=CARTESIAN_POINT('Ctrl Pts',(-1.14543858226948,1.,-1.77313777896234));
#31373=CARTESIAN_POINT('Ctrl Pts',(-1.15090197841531,1.,-1.77627422557034));
#31374=CARTESIAN_POINT('Ctrl Pts',(-1.15639547194689,1.,-1.77938085564261));
#31375=CARTESIAN_POINT('Ctrl Pts',(-1.16191881298458,1.,-1.78245795880949));
#31376=CARTESIAN_POINT('Ctrl Pts',(-1.16747166312239,1.,-1.78550566040349));
#31377=CARTESIAN_POINT('Ctrl Pts',(-1.17305363177265,1.,-1.78852398877523));
#31378=CARTESIAN_POINT('Ctrl Pts',(-1.17866429440781,1.,-1.79151291552646));
#31379=CARTESIAN_POINT('Ctrl Pts',(-1.18430321697471,1.,-1.79447240321572));
#31380=CARTESIAN_POINT('Ctrl Pts',(-1.1899699793456,1.,-1.79740245923649));
#31381=CARTESIAN_POINT('Ctrl Pts',(-1.19566418930405,1.,-1.80030314370121));
#31382=CARTESIAN_POINT('Ctrl Pts',(-1.2013854893912,1.,-1.8031745483882));
#31383=CARTESIAN_POINT('Ctrl Pts',(-1.20713356605519,1.,-1.80601678480772));
#31384=CARTESIAN_POINT('Ctrl Pts',(-1.2129081570818,1.,-1.80882996916931));
#31385=CARTESIAN_POINT('Ctrl Pts',(-1.2187090610323,1.,-1.81161420806172));
#31386=CARTESIAN_POINT('Ctrl Pts',(-1.22453613304507,1.,-1.81436959209778));
#31387=CARTESIAN_POINT('Ctrl Pts',(-1.22921864890975,1.,-1.81655087183054));
#31388=CARTESIAN_POINT('Ctrl Pts',(-1.23274224526804,1.,-1.81817389920914));
#31389=CARTESIAN_POINT('Ctrl Pts',(-1.23509651170384,1.,-1.81925017193531));
#31390=CARTESIAN_POINT('Ctrl Pts',(-1.23627494547115,1.,-1.81978687191668));
#31391=CARTESIAN_POINT('',(-0.892032620296856,0.,-1.5055822144029));
#31392=CARTESIAN_POINT('Origin',(0.,0.,0.));
#31393=CARTESIAN_POINT('',(-0.693717979106305,1.,-1.60662857109684));
#31394=CARTESIAN_POINT('Origin',(0.,1.,0.));
#31395=CARTESIAN_POINT('',(-0.693717979106306,0.,-1.60662857109684));
#31396=CARTESIAN_POINT('Ctrl Pts',(-0.745574324794401,-1.,-2.0698113262342));
#31397=CARTESIAN_POINT('Ctrl Pts',(-0.745574324794401,1.,-2.0698113262342));
#31398=CARTESIAN_POINT('Ctrl Pts',(-0.745832791378367,-1.,-2.06854248895728));
#31399=CARTESIAN_POINT('Ctrl Pts',(-0.745832791378367,1.,-2.06854248895728));
#31400=CARTESIAN_POINT('Ctrl Pts',(-0.7463458715442,-1.,-2.06600523016815));
#31401=CARTESIAN_POINT('Ctrl Pts',(-0.7463458715442,1.,-2.06600523016815));
#31402=CARTESIAN_POINT('Ctrl Pts',(-0.747103932787919,-1.,-2.06220058927826));
#31403=CARTESIAN_POINT('Ctrl Pts',(-0.747103932787919,1.,-2.06220058927826));
#31404=CARTESIAN_POINT('Ctrl Pts',(-0.748091554183802,-1.,-2.05713023031006));
#31405=CARTESIAN_POINT('Ctrl Pts',(-0.748091554183802,1.,-2.05713023031006));
#31406=CARTESIAN_POINT('Ctrl Pts',(-0.749287468665046,-1.,-2.05079645592154));
#31407=CARTESIAN_POINT('Ctrl Pts',(-0.749287468665046,1.,-2.05079645592154));
#31408=CARTESIAN_POINT('Ctrl Pts',(-0.750444657875576,-1.,-2.04446689147979));
#31409=CARTESIAN_POINT('Ctrl Pts',(-0.750444657875576,1.,-2.04446689147979));
#31410=CARTESIAN_POINT('Ctrl Pts',(-0.751562963361115,-1.,-2.03814160092099));
#31411=CARTESIAN_POINT('Ctrl Pts',(-0.751562963361115,1.,-2.03814160092099));
#31412=CARTESIAN_POINT('Ctrl Pts',(-0.752642180487211,-1.,-2.03182068456221));
#31413=CARTESIAN_POINT('Ctrl Pts',(-0.752642180487211,1.,-2.03182068456221));
#31414=CARTESIAN_POINT('Ctrl Pts',(-0.753682061112768,-1.,-2.02550428623313));
#31415=CARTESIAN_POINT('Ctrl Pts',(-0.753682061112768,1.,-2.02550428623313));
#31416=CARTESIAN_POINT('Ctrl Pts',(-0.754682330722816,-1.,-2.01919259405809));
#31417=CARTESIAN_POINT('Ctrl Pts',(-0.754682330722816,1.,-2.01919259405809));
#31418=CARTESIAN_POINT('Ctrl Pts',(-0.755642704957865,-1.,-2.01288584328084));
#31419=CARTESIAN_POINT('Ctrl Pts',(-0.755642704957865,1.,-2.01288584328084));
#31420=CARTESIAN_POINT('Ctrl Pts',(-0.75656290464667,-1.,-2.0065843158773));
#31421=CARTESIAN_POINT('Ctrl Pts',(-0.75656290464667,1.,-2.0065843158773));
#31422=CARTESIAN_POINT('Ctrl Pts',(-0.757442676862724,-1.,-2.00028834739178));
#31423=CARTESIAN_POINT('Ctrl Pts',(-0.757442676862724,1.,-2.00028834739178));
#31424=CARTESIAN_POINT('Ctrl Pts',(-0.758281796766761,-1.,-1.99399831098817));
#31425=CARTESIAN_POINT('Ctrl Pts',(-0.758281796766761,1.,-1.99399831098817));
#31426=CARTESIAN_POINT('Ctrl Pts',(-0.759080037802488,-1.,-1.98771456680874));
#31427=CARTESIAN_POINT('Ctrl Pts',(-0.759080037802488,1.,-1.98771456680874));
#31428=CARTESIAN_POINT('Ctrl Pts',(-0.75983714745219,-1.,-1.98143741418172));
#31429=CARTESIAN_POINT('Ctrl Pts',(-0.75983714745219,1.,-1.98143741418172));
#31430=CARTESIAN_POINT('Ctrl Pts',(-0.760552825409757,-1.,-1.97516705321494));
#31431=CARTESIAN_POINT('Ctrl Pts',(-0.760552825409757,1.,-1.97516705321494));
#31432=CARTESIAN_POINT('Ctrl Pts',(-0.76122669048382,-1.,-1.96890351582499));
#31433=CARTESIAN_POINT('Ctrl Pts',(-0.76122669048382,1.,-1.96890351582499));
#31434=CARTESIAN_POINT('Ctrl Pts',(-0.761858300014423,-1.,-1.96264672744186));
#31435=CARTESIAN_POINT('Ctrl Pts',(-0.761858300014423,1.,-1.96264672744186));
#31436=CARTESIAN_POINT('Ctrl Pts',(-0.762447203806179,-1.,-1.95639665309869));
#31437=CARTESIAN_POINT('Ctrl Pts',(-0.762447203806179,1.,-1.95639665309869));
#31438=CARTESIAN_POINT('Ctrl Pts',(-0.762992990878769,-1.,-1.95015342590024));
#31439=CARTESIAN_POINT('Ctrl Pts',(-0.762992990878769,1.,-1.95015342590024));
#31440=CARTESIAN_POINT('Ctrl Pts',(-0.763495333538629,-1.,-1.9439174661764));
#31441=CARTESIAN_POINT('Ctrl Pts',(-0.763495333538629,1.,-1.9439174661764));
#31442=CARTESIAN_POINT('Ctrl Pts',(-0.763954049121458,-1.,-1.93768964875886));
#31443=CARTESIAN_POINT('Ctrl Pts',(-0.763954049121458,1.,-1.93768964875886));
#31444=CARTESIAN_POINT('Ctrl Pts',(-0.764369010673941,-1.,-1.93147105496382));
#31445=CARTESIAN_POINT('Ctrl Pts',(-0.764369010673941,1.,-1.93147105496382));
#31446=CARTESIAN_POINT('Ctrl Pts',(-0.764740025488211,-1.,-1.92526263537048));
#31447=CARTESIAN_POINT('Ctrl Pts',(-0.764740025488211,1.,-1.92526263537048));
#31448=CARTESIAN_POINT('Ctrl Pts',(-0.765066729667088,-1.,-1.91906491634196));
#31449=CARTESIAN_POINT('Ctrl Pts',(-0.765066729667088,1.,-1.91906491634196));
#31450=CARTESIAN_POINT('Ctrl Pts',(-0.765348465884722,-1.,-1.91287765805169));
#31451=CARTESIAN_POINT('Ctrl Pts',(-0.765348465884722,1.,-1.91287765805169));
#31452=CARTESIAN_POINT('Ctrl Pts',(-0.765584196937919,-1.,-1.90669961402356));
#31453=CARTESIAN_POINT('Ctrl Pts',(-0.765584196937919,1.,-1.90669961402356));
#31454=CARTESIAN_POINT('Ctrl Pts',(-0.765772772593386,-1.,-1.90052930393596));
#31455=CARTESIAN_POINT('Ctrl Pts',(-0.765772772593386,1.,-1.90052930393596));
#31456=CARTESIAN_POINT('Ctrl Pts',(-0.765913193856978,-1.,-1.89436577771388));
#31457=CARTESIAN_POINT('Ctrl Pts',(-0.765913193856978,1.,-1.89436577771388));
#31458=CARTESIAN_POINT('Ctrl Pts',(-0.766004837062091,-1.,-1.88820926433409));
#31459=CARTESIAN_POINT('Ctrl Pts',(-0.766004837062091,1.,-1.88820926433409));
#31460=CARTESIAN_POINT('Ctrl Pts',(-0.766047794851865,-1.,-1.88206215302561));
#31461=CARTESIAN_POINT('Ctrl Pts',(-0.766047794851865,1.,-1.88206215302561));
#31462=CARTESIAN_POINT('Ctrl Pts',(-0.766042837036744,-1.,-1.87592888967883));
#31463=CARTESIAN_POINT('Ctrl Pts',(-0.766042837036744,1.,-1.87592888967883));
#31464=CARTESIAN_POINT('Ctrl Pts',(-0.765990708546091,-1.,-1.86981398314341));
#31465=CARTESIAN_POINT('Ctrl Pts',(-0.765990708546091,1.,-1.86981398314341));
#31466=CARTESIAN_POINT('Ctrl Pts',(-0.765891519092547,-1.,-1.86372027063312));
#31467=CARTESIAN_POINT('Ctrl Pts',(-0.765891519092547,1.,-1.86372027063312));
#31468=CARTESIAN_POINT('Ctrl Pts',(-0.765744212909318,-1.,-1.85764741390394));
#31469=CARTESIAN_POINT('Ctrl Pts',(-0.765744212909318,1.,-1.85764741390394));
#31470=CARTESIAN_POINT('Ctrl Pts',(-0.765545710619062,-1.,-1.85158945130063));
#31471=CARTESIAN_POINT('Ctrl Pts',(-0.765545710619062,1.,-1.85158945130063));
#31472=CARTESIAN_POINT('Ctrl Pts',(-0.765291664862029,-1.,-1.84553698875924));
#31473=CARTESIAN_POINT('Ctrl Pts',(-0.765291664862029,1.,-1.84553698875924));
#31474=CARTESIAN_POINT('Ctrl Pts',(-0.764978057881737,-1.,-1.83948181064835));
#31475=CARTESIAN_POINT('Ctrl Pts',(-0.764978057881737,1.,-1.83948181064835));
#31476=CARTESIAN_POINT('Ctrl Pts',(-0.764602549687853,-1.,-1.83342077227142));
#31477=CARTESIAN_POINT('Ctrl Pts',(-0.764602549687853,1.,-1.83342077227142));
#31478=CARTESIAN_POINT('Ctrl Pts',(-0.764165902605995,-1.,-1.82735991200065));
#31479=CARTESIAN_POINT('Ctrl Pts',(-0.764165902605995,1.,-1.82735991200065));
#31480=CARTESIAN_POINT('Ctrl Pts',(-0.763673465462726,-1.,-1.82131873145266));
#31481=CARTESIAN_POINT('Ctrl Pts',(-0.763673465462726,1.,-1.82131873145266));
#31482=CARTESIAN_POINT('Ctrl Pts',(-0.763132003836634,-1.,-1.8153211840553));
#31483=CARTESIAN_POINT('Ctrl Pts',(-0.763132003836634,1.,-1.8153211840553));
#31484=CARTESIAN_POINT('Ctrl Pts',(-0.762546129463938,-1.,-1.80938551463965));
#31485=CARTESIAN_POINT('Ctrl Pts',(-0.762546129463938,1.,-1.80938551463965));
#31486=CARTESIAN_POINT('Ctrl Pts',(-0.761915336443547,-1.,-1.80351583877342));
#31487=CARTESIAN_POINT('Ctrl Pts',(-0.761915336443547,1.,-1.80351583877342));
#31488=CARTESIAN_POINT('Ctrl Pts',(-0.761229695230558,-1.,-1.79768986997783));
#31489=CARTESIAN_POINT('Ctrl Pts',(-0.761229695230558,1.,-1.79768986997783));
#31490=CARTESIAN_POINT('Ctrl Pts',(-0.760469555880749,-1.,-1.7918581561088));
#31491=CARTESIAN_POINT('Ctrl Pts',(-0.760469555880749,1.,-1.7918581561088));
#31492=CARTESIAN_POINT('Ctrl Pts',(-0.759614401110189,-1.,-1.78596964884604));
#31493=CARTESIAN_POINT('Ctrl Pts',(-0.759614401110189,1.,-1.78596964884604));
#31494=CARTESIAN_POINT('Ctrl Pts',(-0.758650626677518,-1.,-1.77999411220945));
#31495=CARTESIAN_POINT('Ctrl Pts',(-0.758650626677518,1.,-1.77999411220945));
#31496=CARTESIAN_POINT('Ctrl Pts',(-0.757578264077029,-1.,-1.77394167108292));
#31497=CARTESIAN_POINT('Ctrl Pts',(-0.757578264077029,1.,-1.77394167108292));
#31498=CARTESIAN_POINT('Ctrl Pts',(-0.75642189602781,-1.,-1.76789396002998));
#31499=CARTESIAN_POINT('Ctrl Pts',(-0.75642189602781,1.,-1.76789396002998));
#31500=CARTESIAN_POINT('Ctrl Pts',(-0.755220979974461,-1.,-1.76197817240128));
#31501=CARTESIAN_POINT('Ctrl Pts',(-0.755220979974461,1.,-1.76197817240128));
#31502=CARTESIAN_POINT('Ctrl Pts',(-0.754009254027829,-1.,-1.75631083600019));
#31503=CARTESIAN_POINT('Ctrl Pts',(-0.754009254027829,1.,-1.75631083600019));
#31504=CARTESIAN_POINT('Ctrl Pts',(-0.752797683531314,-1.,-1.75095139468794));
#31505=CARTESIAN_POINT('Ctrl Pts',(-0.752797683531314,1.,-1.75095139468794));
#31506=CARTESIAN_POINT('Ctrl Pts',(-0.751555614164482,-1.,-1.74585086852502));
#31507=CARTESIAN_POINT('Ctrl Pts',(-0.751555614164482,1.,-1.74585086852502));
#31508=CARTESIAN_POINT('Ctrl Pts',(-0.750193435981249,-1.,-1.74080458267114));
#31509=CARTESIAN_POINT('Ctrl Pts',(-0.750193435981249,1.,-1.74080458267114));
#31510=CARTESIAN_POINT('Ctrl Pts',(-0.74858246295687,-1.,-1.7355035168033));
#31511=CARTESIAN_POINT('Ctrl Pts',(-0.74858246295687,1.,-1.7355035168033));
#31512=CARTESIAN_POINT('Ctrl Pts',(-0.746574710097752,-1.,-1.72958533647714));
#31513=CARTESIAN_POINT('Ctrl Pts',(-0.746574710097752,1.,-1.72958533647714));
#31514=CARTESIAN_POINT('Ctrl Pts',(-0.744021445433093,-1.,-1.72268229916769));
#31515=CARTESIAN_POINT('Ctrl Pts',(-0.744021445433093,1.,-1.72268229916769));
#31516=CARTESIAN_POINT('Ctrl Pts',(-0.74079516202821,-1.,-1.71447789751001));
#31517=CARTESIAN_POINT('Ctrl Pts',(-0.74079516202821,1.,-1.71447789751001));
#31518=CARTESIAN_POINT('Ctrl Pts',(-0.736799665716932,-1.,-1.70473309004249));
#31519=CARTESIAN_POINT('Ctrl Pts',(-0.736799665716932,1.,-1.70473309004249));
#31520=CARTESIAN_POINT('Ctrl Pts',(-0.731963238685357,-1.,-1.69326921972915));
#31521=CARTESIAN_POINT('Ctrl Pts',(-0.731963238685357,1.,-1.69326921972915));
#31522=CARTESIAN_POINT('Ctrl Pts',(-0.726235967982445,-1.,-1.67996158451922));
#31523=CARTESIAN_POINT('Ctrl Pts',(-0.726235967982445,1.,-1.67996158451922));
#31524=CARTESIAN_POINT('Ctrl Pts',(-0.71958543378795,-1.,-1.66472880551777));
#31525=CARTESIAN_POINT('Ctrl Pts',(-0.71958543378795,1.,-1.66472880551777));
#31526=CARTESIAN_POINT('Ctrl Pts',(-0.711993139340447,-1.,-1.64752408828442));
#31527=CARTESIAN_POINT('Ctrl Pts',(-0.711993139340447,1.,-1.64752408828442));
#31528=CARTESIAN_POINT('Ctrl Pts',(-0.705159151977294,-1.,-1.6321654166204));
#31529=CARTESIAN_POINT('Ctrl Pts',(-0.705159151977294,1.,-1.6321654166204));
#31530=CARTESIAN_POINT('Ctrl Pts',(-0.699605146398837,-1.,-1.61974673471117));
#31531=CARTESIAN_POINT('Ctrl Pts',(-0.699605146398837,1.,-1.61974673471117));
#31532=CARTESIAN_POINT('Ctrl Pts',(-0.69571209787897,-1.,-1.61106790957619));
#31533=CARTESIAN_POINT('Ctrl Pts',(-0.69571209787897,1.,-1.61106790957619));
#31534=CARTESIAN_POINT('Ctrl Pts',(-0.693717979106305,-1.,-1.60662857109684));
#31535=CARTESIAN_POINT('Ctrl Pts',(-0.693717979106305,1.,-1.60662857109684));
#31536=CARTESIAN_POINT('',(-0.745574324794401,1.,-2.0698113262342));
#31537=CARTESIAN_POINT('Ctrl Pts',(-0.745574324794401,1.,-2.0698113262342));
#31538=CARTESIAN_POINT('Ctrl Pts',(-0.745832791378367,1.,-2.06854248895728));
#31539=CARTESIAN_POINT('Ctrl Pts',(-0.7463458715442,1.,-2.06600523016815));
#31540=CARTESIAN_POINT('Ctrl Pts',(-0.747103932787919,1.,-2.06220058927826));
#31541=CARTESIAN_POINT('Ctrl Pts',(-0.748091554183802,1.,-2.05713023031006));
#31542=CARTESIAN_POINT('Ctrl Pts',(-0.749287468665046,1.,-2.05079645592154));
#31543=CARTESIAN_POINT('Ctrl Pts',(-0.750444657875576,1.,-2.04446689147979));
#31544=CARTESIAN_POINT('Ctrl Pts',(-0.751562963361115,1.,-2.03814160092099));
#31545=CARTESIAN_POINT('Ctrl Pts',(-0.752642180487211,1.,-2.03182068456221));
#31546=CARTESIAN_POINT('Ctrl Pts',(-0.753682061112768,1.,-2.02550428623313));
#31547=CARTESIAN_POINT('Ctrl Pts',(-0.754682330722816,1.,-2.01919259405809));
#31548=CARTESIAN_POINT('Ctrl Pts',(-0.755642704957865,1.,-2.01288584328084));
#31549=CARTESIAN_POINT('Ctrl Pts',(-0.75656290464667,1.,-2.0065843158773));
#31550=CARTESIAN_POINT('Ctrl Pts',(-0.757442676862724,1.,-2.00028834739178));
#31551=CARTESIAN_POINT('Ctrl Pts',(-0.758281796766761,1.,-1.99399831098817));
#31552=CARTESIAN_POINT('Ctrl Pts',(-0.759080037802488,1.,-1.98771456680874));
#31553=CARTESIAN_POINT('Ctrl Pts',(-0.75983714745219,1.,-1.98143741418172));
#31554=CARTESIAN_POINT('Ctrl Pts',(-0.760552825409757,1.,-1.97516705321494));
#31555=CARTESIAN_POINT('Ctrl Pts',(-0.76122669048382,1.,-1.96890351582499));
#31556=CARTESIAN_POINT('Ctrl Pts',(-0.761858300014423,1.,-1.96264672744186));
#31557=CARTESIAN_POINT('Ctrl Pts',(-0.762447203806179,1.,-1.95639665309869));
#31558=CARTESIAN_POINT('Ctrl Pts',(-0.762992990878769,1.,-1.95015342590024));
#31559=CARTESIAN_POINT('Ctrl Pts',(-0.763495333538629,1.,-1.9439174661764));
#31560=CARTESIAN_POINT('Ctrl Pts',(-0.763954049121458,1.,-1.93768964875886));
#31561=CARTESIAN_POINT('Ctrl Pts',(-0.764369010673941,1.,-1.93147105496382));
#31562=CARTESIAN_POINT('Ctrl Pts',(-0.764740025488211,1.,-1.92526263537048));
#31563=CARTESIAN_POINT('Ctrl Pts',(-0.765066729667088,1.,-1.91906491634196));
#31564=CARTESIAN_POINT('Ctrl Pts',(-0.765348465884722,1.,-1.91287765805169));
#31565=CARTESIAN_POINT('Ctrl Pts',(-0.765584196937919,1.,-1.90669961402356));
#31566=CARTESIAN_POINT('Ctrl Pts',(-0.765772772593386,1.,-1.90052930393596));
#31567=CARTESIAN_POINT('Ctrl Pts',(-0.765913193856978,1.,-1.89436577771388));
#31568=CARTESIAN_POINT('Ctrl Pts',(-0.766004837062091,1.,-1.88820926433409));
#31569=CARTESIAN_POINT('Ctrl Pts',(-0.766047794851865,1.,-1.88206215302561));
#31570=CARTESIAN_POINT('Ctrl Pts',(-0.766042837036744,1.,-1.87592888967883));
#31571=CARTESIAN_POINT('Ctrl Pts',(-0.765990708546091,1.,-1.86981398314341));
#31572=CARTESIAN_POINT('Ctrl Pts',(-0.765891519092547,1.,-1.86372027063312));
#31573=CARTESIAN_POINT('Ctrl Pts',(-0.765744212909318,1.,-1.85764741390394));
#31574=CARTESIAN_POINT('Ctrl Pts',(-0.765545710619062,1.,-1.85158945130063));
#31575=CARTESIAN_POINT('Ctrl Pts',(-0.765291664862029,1.,-1.84553698875924));
#31576=CARTESIAN_POINT('Ctrl Pts',(-0.764978057881737,1.,-1.83948181064835));
#31577=CARTESIAN_POINT('Ctrl Pts',(-0.764602549687853,1.,-1.83342077227142));
#31578=CARTESIAN_POINT('Ctrl Pts',(-0.764165902605995,1.,-1.82735991200065));
#31579=CARTESIAN_POINT('Ctrl Pts',(-0.763673465462726,1.,-1.82131873145266));
#31580=CARTESIAN_POINT('Ctrl Pts',(-0.763132003836634,1.,-1.8153211840553));
#31581=CARTESIAN_POINT('Ctrl Pts',(-0.762546129463938,1.,-1.80938551463965));
#31582=CARTESIAN_POINT('Ctrl Pts',(-0.761915336443547,1.,-1.80351583877342));
#31583=CARTESIAN_POINT('Ctrl Pts',(-0.761229695230558,1.,-1.79768986997783));
#31584=CARTESIAN_POINT('Ctrl Pts',(-0.760469555880749,1.,-1.7918581561088));
#31585=CARTESIAN_POINT('Ctrl Pts',(-0.759614401110189,1.,-1.78596964884604));
#31586=CARTESIAN_POINT('Ctrl Pts',(-0.758650626677518,1.,-1.77999411220945));
#31587=CARTESIAN_POINT('Ctrl Pts',(-0.757578264077029,1.,-1.77394167108292));
#31588=CARTESIAN_POINT('Ctrl Pts',(-0.75642189602781,1.,-1.76789396002998));
#31589=CARTESIAN_POINT('Ctrl Pts',(-0.755220979974461,1.,-1.76197817240128));
#31590=CARTESIAN_POINT('Ctrl Pts',(-0.754009254027829,1.,-1.75631083600019));
#31591=CARTESIAN_POINT('Ctrl Pts',(-0.752797683531314,1.,-1.75095139468794));
#31592=CARTESIAN_POINT('Ctrl Pts',(-0.751555614164482,1.,-1.74585086852502));
#31593=CARTESIAN_POINT('Ctrl Pts',(-0.750193435981249,1.,-1.74080458267114));
#31594=CARTESIAN_POINT('Ctrl Pts',(-0.74858246295687,1.,-1.7355035168033));
#31595=CARTESIAN_POINT('Ctrl Pts',(-0.746574710097752,1.,-1.72958533647714));
#31596=CARTESIAN_POINT('Ctrl Pts',(-0.744021445433093,1.,-1.72268229916769));
#31597=CARTESIAN_POINT('Ctrl Pts',(-0.74079516202821,1.,-1.71447789751001));
#31598=CARTESIAN_POINT('Ctrl Pts',(-0.736799665716932,1.,-1.70473309004249));
#31599=CARTESIAN_POINT('Ctrl Pts',(-0.731963238685357,1.,-1.69326921972915));
#31600=CARTESIAN_POINT('Ctrl Pts',(-0.726235967982445,1.,-1.67996158451922));
#31601=CARTESIAN_POINT('Ctrl Pts',(-0.71958543378795,1.,-1.66472880551777));
#31602=CARTESIAN_POINT('Ctrl Pts',(-0.711993139340447,1.,-1.64752408828442));
#31603=CARTESIAN_POINT('Ctrl Pts',(-0.705159151977294,1.,-1.6321654166204));
#31604=CARTESIAN_POINT('Ctrl Pts',(-0.699605146398837,1.,-1.61974673471117));
#31605=CARTESIAN_POINT('Ctrl Pts',(-0.69571209787897,1.,-1.61106790957619));
#31606=CARTESIAN_POINT('Ctrl Pts',(-0.693717979106305,1.,-1.60662857109684));
#31607=CARTESIAN_POINT('',(-0.745574324794401,0.,-2.0698113262342));
#31608=CARTESIAN_POINT('Origin',(-0.61342227326009,0.,-2.11275013067528));
#31609=CARTESIAN_POINT('',(-0.61342227326009,1.,-2.11275013067528));
#31610=CARTESIAN_POINT('',(-0.745574324794401,1.,-2.0698113262342));
#31611=CARTESIAN_POINT('',(-0.61342227326009,0.,-2.11275013067528));
#31612=CARTESIAN_POINT('Ctrl Pts',(-0.383122945602004,-1.,-1.7075470150345));
#31613=CARTESIAN_POINT('Ctrl Pts',(-0.383122945602004,1.,-1.7075470150345));
#31614=CARTESIAN_POINT('Ctrl Pts',(-0.384119047315542,-1.,-1.71231062891958));
#31615=CARTESIAN_POINT('Ctrl Pts',(-0.384119047315542,1.,-1.71231062891958));
#31616=CARTESIAN_POINT('Ctrl Pts',(-0.38607079032701,-1.,-1.72162022246158));
#31617=CARTESIAN_POINT('Ctrl Pts',(-0.38607079032701,1.,-1.72162022246158));
#31618=CARTESIAN_POINT('Ctrl Pts',(-0.388877023509191,-1.,-1.7349317097561));
#31619=CARTESIAN_POINT('Ctrl Pts',(-0.388877023509191,1.,-1.7349317097561));
#31620=CARTESIAN_POINT('Ctrl Pts',(-0.392375812294307,-1.,-1.75137405313962));
#31621=CARTESIAN_POINT('Ctrl Pts',(-0.392375812294307,1.,-1.75137405313962));
#31622=CARTESIAN_POINT('Ctrl Pts',(-0.39634619612042,-1.,-1.7697556004756));
#31623=CARTESIAN_POINT('Ctrl Pts',(-0.39634619612042,1.,-1.7697556004756));
#31624=CARTESIAN_POINT('Ctrl Pts',(-0.39991940378308,-1.,-1.78598826347533));
#31625=CARTESIAN_POINT('Ctrl Pts',(-0.39991940378308,1.,-1.78598826347533));
#31626=CARTESIAN_POINT('Ctrl Pts',(-0.403107976170441,-1.,-1.80012077176221));
#31627=CARTESIAN_POINT('Ctrl Pts',(-0.403107976170441,1.,-1.80012077176221));
#31628=CARTESIAN_POINT('Ctrl Pts',(-0.405933518411838,-1.,-1.81223801813988));
#31629=CARTESIAN_POINT('Ctrl Pts',(-0.405933518411838,1.,-1.81223801813988));
#31630=CARTESIAN_POINT('Ctrl Pts',(-0.408428948108533,-1.,-1.8224702267854));
#31631=CARTESIAN_POINT('Ctrl Pts',(-0.408428948108533,1.,-1.8224702267854));
#31632=CARTESIAN_POINT('Ctrl Pts',(-0.410641256301675,-1.,-1.83100408895216));
#31633=CARTESIAN_POINT('Ctrl Pts',(-0.410641256301675,1.,-1.83100408895216));
#31634=CARTESIAN_POINT('Ctrl Pts',(-0.412633125322162,-1.,-1.83808953475839));
#31635=CARTESIAN_POINT('Ctrl Pts',(-0.412633125322162,1.,-1.83808953475839));
#31636=CARTESIAN_POINT('Ctrl Pts',(-0.41448743825434,-1.,-1.8440575707371));
#31637=CARTESIAN_POINT('Ctrl Pts',(-0.41448743825434,1.,-1.8440575707371));
#31638=CARTESIAN_POINT('Ctrl Pts',(-0.416300022038864,-1.,-1.84929312929882));
#31639=CARTESIAN_POINT('Ctrl Pts',(-0.416300022038864,1.,-1.84929312929882));
#31640=CARTESIAN_POINT('Ctrl Pts',(-0.418164129143534,-1.,-1.85417632856234));
#31641=CARTESIAN_POINT('Ctrl Pts',(-0.418164129143534,1.,-1.85417632856234));
#31642=CARTESIAN_POINT('Ctrl Pts',(-0.420157287975619,-1.,-1.85903281096686));
#31643=CARTESIAN_POINT('Ctrl Pts',(-0.420157287975619,1.,-1.85903281096686));
#31644=CARTESIAN_POINT('Ctrl Pts',(-0.422327307418275,-1.,-1.86408083334028));
#31645=CARTESIAN_POINT('Ctrl Pts',(-0.422327307418275,1.,-1.86408083334028));
#31646=CARTESIAN_POINT('Ctrl Pts',(-0.424678177291359,-1.,-1.86937803944323));
#31647=CARTESIAN_POINT('Ctrl Pts',(-0.424678177291359,1.,-1.86937803944323));
#31648=CARTESIAN_POINT('Ctrl Pts',(-0.427183828519102,-1.,-1.87486989291484));
#31649=CARTESIAN_POINT('Ctrl Pts',(-0.427183828519102,1.,-1.87486989291484));
#31650=CARTESIAN_POINT('Ctrl Pts',(-0.429803062482344,-1.,-1.88044229001832));
#31651=CARTESIAN_POINT('Ctrl Pts',(-0.429803062482344,1.,-1.88044229001832));
#31652=CARTESIAN_POINT('Ctrl Pts',(-0.432493038548748,-1.,-1.88596913666793));
#31653=CARTESIAN_POINT('Ctrl Pts',(-0.432493038548748,1.,-1.88596913666793));
#31654=CARTESIAN_POINT('Ctrl Pts',(-0.435225660963383,-1.,-1.89136993975504));
#31655=CARTESIAN_POINT('Ctrl Pts',(-0.435225660963383,1.,-1.89136993975504));
#31656=CARTESIAN_POINT('Ctrl Pts',(-0.437995003948244,-1.,-1.89663648956466));
#31657=CARTESIAN_POINT('Ctrl Pts',(-0.437995003948244,1.,-1.89663648956466));
#31658=CARTESIAN_POINT('Ctrl Pts',(-0.440807833704038,-1.,-1.90180124389086));
#31659=CARTESIAN_POINT('Ctrl Pts',(-0.440807833704038,1.,-1.90180124389086));
#31660=CARTESIAN_POINT('Ctrl Pts',(-0.443677556849151,-1.,-1.90691756144898));
#31661=CARTESIAN_POINT('Ctrl Pts',(-0.443677556849151,1.,-1.90691756144898));
#31662=CARTESIAN_POINT('Ctrl Pts',(-0.446617343485711,-1.,-1.9120369998112));
#31663=CARTESIAN_POINT('Ctrl Pts',(-0.446617343485711,1.,-1.9120369998112));
#31664=CARTESIAN_POINT('Ctrl Pts',(-0.449632260106662,-1.,-1.91718342555755));
#31665=CARTESIAN_POINT('Ctrl Pts',(-0.449632260106662,1.,-1.91718342555755));
#31666=CARTESIAN_POINT('Ctrl Pts',(-0.452719478359432,-1.,-1.92235380648502));
#31667=CARTESIAN_POINT('Ctrl Pts',(-0.452719478359432,1.,-1.92235380648502));
#31668=CARTESIAN_POINT('Ctrl Pts',(-0.455872005174371,-1.,-1.92753067150476));
#31669=CARTESIAN_POINT('Ctrl Pts',(-0.455872005174371,1.,-1.92753067150476));
#31670=CARTESIAN_POINT('Ctrl Pts',(-0.459081234547926,-1.,-1.93269066517934));
#31671=CARTESIAN_POINT('Ctrl Pts',(-0.459081234547926,1.,-1.93269066517934));
#31672=CARTESIAN_POINT('Ctrl Pts',(-0.462340031009056,-1.,-1.93781486640821));
#31673=CARTESIAN_POINT('Ctrl Pts',(-0.462340031009056,1.,-1.93781486640821));
#31674=CARTESIAN_POINT('Ctrl Pts',(-0.46564546202603,-1.,-1.9428979419619));
#31675=CARTESIAN_POINT('Ctrl Pts',(-0.46564546202603,1.,-1.9428979419619));
#31676=CARTESIAN_POINT('Ctrl Pts',(-0.468997482913135,-1.,-1.94794381136514));
#31677=CARTESIAN_POINT('Ctrl Pts',(-0.468997482913135,1.,-1.94794381136514));
#31678=CARTESIAN_POINT('Ctrl Pts',(-0.472397672264072,-1.,-1.95296148278133));
#31679=CARTESIAN_POINT('Ctrl Pts',(-0.472397672264072,1.,-1.95296148278133));
#31680=CARTESIAN_POINT('Ctrl Pts',(-0.475848034683176,-1.,-1.95796111148177));
#31681=CARTESIAN_POINT('Ctrl Pts',(-0.475848034683176,1.,-1.95796111148177));
#31682=CARTESIAN_POINT('Ctrl Pts',(-0.479349583074855,-1.,-1.96294933055943));
#31683=CARTESIAN_POINT('Ctrl Pts',(-0.479349583074855,1.,-1.96294933055943));
#31684=CARTESIAN_POINT('Ctrl Pts',(-0.482901662120691,-1.,-1.96792703422362));
#31685=CARTESIAN_POINT('Ctrl Pts',(-0.482901662120691,1.,-1.96792703422362));
#31686=CARTESIAN_POINT('Ctrl Pts',(-0.486502692907659,-1.,-1.97289186263272));
#31687=CARTESIAN_POINT('Ctrl Pts',(-0.486502692907659,1.,-1.97289186263272));
#31688=CARTESIAN_POINT('Ctrl Pts',(-0.490150627860952,-1.,-1.97783973019229));
#31689=CARTESIAN_POINT('Ctrl Pts',(-0.490150627860952,1.,-1.97783973019229));
#31690=CARTESIAN_POINT('Ctrl Pts',(-0.493843476541495,-1.,-1.98276658761821));
#31691=CARTESIAN_POINT('Ctrl Pts',(-0.493843476541495,1.,-1.98276658761821));
#31692=CARTESIAN_POINT('Ctrl Pts',(-0.497579909545574,-1.,-1.98767044752932));
#31693=CARTESIAN_POINT('Ctrl Pts',(-0.497579909545574,1.,-1.98767044752932));
#31694=CARTESIAN_POINT('Ctrl Pts',(-0.501359287727146,-1.,-1.99255149126155));
#31695=CARTESIAN_POINT('Ctrl Pts',(-0.501359287727146,1.,-1.99255149126155));
#31696=CARTESIAN_POINT('Ctrl Pts',(-0.505181361323026,-1.,-1.99741107463572));
#31697=CARTESIAN_POINT('Ctrl Pts',(-0.505181361323026,1.,-1.99741107463572));
#31698=CARTESIAN_POINT('Ctrl Pts',(-0.509046069886157,-1.,-2.00225107134734));
#31699=CARTESIAN_POINT('Ctrl Pts',(-0.509046069886157,1.,-2.00225107134734));
#31700=CARTESIAN_POINT('Ctrl Pts',(-0.512953306961792,-1.,-2.00707309946949));
#31701=CARTESIAN_POINT('Ctrl Pts',(-0.512953306961792,1.,-2.00707309946949));
#31702=CARTESIAN_POINT('Ctrl Pts',(-0.516902681728687,-1.,-2.01187773939242));
#31703=CARTESIAN_POINT('Ctrl Pts',(-0.516902681728687,1.,-2.01187773939242));
#31704=CARTESIAN_POINT('Ctrl Pts',(-0.52089359039937,-1.,-2.01666477917286));
#31705=CARTESIAN_POINT('Ctrl Pts',(-0.52089359039937,1.,-2.01666477917286));
#31706=CARTESIAN_POINT('Ctrl Pts',(-0.524925318333476,-1.,-2.02143356304698));
#31707=CARTESIAN_POINT('Ctrl Pts',(-0.524925318333476,1.,-2.02143356304698));
#31708=CARTESIAN_POINT('Ctrl Pts',(-0.528997127241914,-1.,-2.0261832908329));
#31709=CARTESIAN_POINT('Ctrl Pts',(-0.528997127241914,1.,-2.0261832908329));
#31710=CARTESIAN_POINT('Ctrl Pts',(-0.533108355132977,-1.,-2.03091336214426));
#31711=CARTESIAN_POINT('Ctrl Pts',(-0.533108355132977,1.,-2.03091336214426));
#31712=CARTESIAN_POINT('Ctrl Pts',(-0.537258489833262,-1.,-2.03562362954037));
#31713=CARTESIAN_POINT('Ctrl Pts',(-0.537258489833262,1.,-2.03562362954037));
#31714=CARTESIAN_POINT('Ctrl Pts',(-0.541447120615659,-1.,-2.04031422690527));
#31715=CARTESIAN_POINT('Ctrl Pts',(-0.541447120615659,1.,-2.04031422690527));
#31716=CARTESIAN_POINT('Ctrl Pts',(-0.54567390381743,-1.,-2.04498544714588));
#31717=CARTESIAN_POINT('Ctrl Pts',(-0.54567390381743,1.,-2.04498544714588));
#31718=CARTESIAN_POINT('Ctrl Pts',(-0.549938525150295,-1.,-2.04963761077958));
#31719=CARTESIAN_POINT('Ctrl Pts',(-0.549938525150295,1.,-2.04963761077958));
#31720=CARTESIAN_POINT('Ctrl Pts',(-0.554240657463906,-1.,-2.05427091604413));
#31721=CARTESIAN_POINT('Ctrl Pts',(-0.554240657463906,1.,-2.05427091604413));
#31722=CARTESIAN_POINT('Ctrl Pts',(-0.558579940185151,-1.,-2.05888537756462));
#31723=CARTESIAN_POINT('Ctrl Pts',(-0.558579940185151,1.,-2.05888537756462));
#31724=CARTESIAN_POINT('Ctrl Pts',(-0.562955993082261,-1.,-2.06348090160589));
#31725=CARTESIAN_POINT('Ctrl Pts',(-0.562955993082261,1.,-2.06348090160589));
#31726=CARTESIAN_POINT('Ctrl Pts',(-0.567368421181087,-1.,-2.06805732997334));
#31727=CARTESIAN_POINT('Ctrl Pts',(-0.567368421181087,1.,-2.06805732997334));
#31728=CARTESIAN_POINT('Ctrl Pts',(-0.571816823242603,-1.,-2.07261449292824));
#31729=CARTESIAN_POINT('Ctrl Pts',(-0.571816823242603,1.,-2.07261449292824));
#31730=CARTESIAN_POINT('Ctrl Pts',(-0.576300797416844,-1.,-2.07715226767559));
#31731=CARTESIAN_POINT('Ctrl Pts',(-0.576300797416844,1.,-2.07715226767559));
#31732=CARTESIAN_POINT('Ctrl Pts',(-0.580819952108063,-1.,-2.08167059018418));
#31733=CARTESIAN_POINT('Ctrl Pts',(-0.580819952108063,1.,-2.08167059018418));
#31734=CARTESIAN_POINT('Ctrl Pts',(-0.585373918991617,-1.,-2.08616943727951));
#31735=CARTESIAN_POINT('Ctrl Pts',(-0.585373918991617,1.,-2.08616943727951));
#31736=CARTESIAN_POINT('Ctrl Pts',(-0.589962365403406,-1.,-2.09064881812129));
#31737=CARTESIAN_POINT('Ctrl Pts',(-0.589962365403406,1.,-2.09064881812129));
#31738=CARTESIAN_POINT('Ctrl Pts',(-0.594585006052162,-1.,-2.0951087622027));
#31739=CARTESIAN_POINT('Ctrl Pts',(-0.594585006052162,1.,-2.0951087622027));
#31740=CARTESIAN_POINT('Ctrl Pts',(-0.599241616420533,-1.,-2.0995493086477));
#31741=CARTESIAN_POINT('Ctrl Pts',(-0.599241616420533,1.,-2.0995493086477));
#31742=CARTESIAN_POINT('Ctrl Pts',(-0.60393203073603,-1.,-2.10397049886949));
#31743=CARTESIAN_POINT('Ctrl Pts',(-0.60393203073603,1.,-2.10397049886949));
#31744=CARTESIAN_POINT('Ctrl Pts',(-0.607711315454876,-1.,-2.1074919961518));
#31745=CARTESIAN_POINT('Ctrl Pts',(-0.607711315454876,1.,-2.1074919961518));
#31746=CARTESIAN_POINT('Ctrl Pts',(-0.610560911689899,-1.,-2.11012443807238));
#31747=CARTESIAN_POINT('Ctrl Pts',(-0.610560911689899,1.,-2.11012443807238));
#31748=CARTESIAN_POINT('Ctrl Pts',(-0.6124673655618,-1.,-2.11187554259986));
#31749=CARTESIAN_POINT('Ctrl Pts',(-0.6124673655618,1.,-2.11187554259986));
#31750=CARTESIAN_POINT('Ctrl Pts',(-0.61342227326009,-1.,-2.11275013067528));
#31751=CARTESIAN_POINT('Ctrl Pts',(-0.61342227326009,1.,-2.11275013067528));
#31752=CARTESIAN_POINT('',(-0.383122945602004,1.,-1.7075470150345));
#31753=CARTESIAN_POINT('Ctrl Pts',(-0.383122945602004,1.,-1.7075470150345));
#31754=CARTESIAN_POINT('Ctrl Pts',(-0.384119047315542,1.,-1.71231062891958));
#31755=CARTESIAN_POINT('Ctrl Pts',(-0.38607079032701,1.,-1.72162022246158));
#31756=CARTESIAN_POINT('Ctrl Pts',(-0.388877023509191,1.,-1.7349317097561));
#31757=CARTESIAN_POINT('Ctrl Pts',(-0.392375812294307,1.,-1.75137405313962));
#31758=CARTESIAN_POINT('Ctrl Pts',(-0.39634619612042,1.,-1.7697556004756));
#31759=CARTESIAN_POINT('Ctrl Pts',(-0.39991940378308,1.,-1.78598826347533));
#31760=CARTESIAN_POINT('Ctrl Pts',(-0.403107976170441,1.,-1.80012077176221));
#31761=CARTESIAN_POINT('Ctrl Pts',(-0.405933518411838,1.,-1.81223801813988));
#31762=CARTESIAN_POINT('Ctrl Pts',(-0.408428948108533,1.,-1.8224702267854));
#31763=CARTESIAN_POINT('Ctrl Pts',(-0.410641256301675,1.,-1.83100408895216));
#31764=CARTESIAN_POINT('Ctrl Pts',(-0.412633125322162,1.,-1.83808953475839));
#31765=CARTESIAN_POINT('Ctrl Pts',(-0.41448743825434,1.,-1.8440575707371));
#31766=CARTESIAN_POINT('Ctrl Pts',(-0.416300022038864,1.,-1.84929312929882));
#31767=CARTESIAN_POINT('Ctrl Pts',(-0.418164129143534,1.,-1.85417632856234));
#31768=CARTESIAN_POINT('Ctrl Pts',(-0.420157287975619,1.,-1.85903281096686));
#31769=CARTESIAN_POINT('Ctrl Pts',(-0.422327307418275,1.,-1.86408083334028));
#31770=CARTESIAN_POINT('Ctrl Pts',(-0.424678177291359,1.,-1.86937803944323));
#31771=CARTESIAN_POINT('Ctrl Pts',(-0.427183828519102,1.,-1.87486989291484));
#31772=CARTESIAN_POINT('Ctrl Pts',(-0.429803062482344,1.,-1.88044229001832));
#31773=CARTESIAN_POINT('Ctrl Pts',(-0.432493038548748,1.,-1.88596913666793));
#31774=CARTESIAN_POINT('Ctrl Pts',(-0.435225660963383,1.,-1.89136993975504));
#31775=CARTESIAN_POINT('Ctrl Pts',(-0.437995003948244,1.,-1.89663648956466));
#31776=CARTESIAN_POINT('Ctrl Pts',(-0.440807833704038,1.,-1.90180124389086));
#31777=CARTESIAN_POINT('Ctrl Pts',(-0.443677556849151,1.,-1.90691756144898));
#31778=CARTESIAN_POINT('Ctrl Pts',(-0.446617343485711,1.,-1.9120369998112));
#31779=CARTESIAN_POINT('Ctrl Pts',(-0.449632260106662,1.,-1.91718342555755));
#31780=CARTESIAN_POINT('Ctrl Pts',(-0.452719478359432,1.,-1.92235380648502));
#31781=CARTESIAN_POINT('Ctrl Pts',(-0.455872005174371,1.,-1.92753067150476));
#31782=CARTESIAN_POINT('Ctrl Pts',(-0.459081234547926,1.,-1.93269066517934));
#31783=CARTESIAN_POINT('Ctrl Pts',(-0.462340031009056,1.,-1.93781486640821));
#31784=CARTESIAN_POINT('Ctrl Pts',(-0.46564546202603,1.,-1.9428979419619));
#31785=CARTESIAN_POINT('Ctrl Pts',(-0.468997482913135,1.,-1.94794381136514));
#31786=CARTESIAN_POINT('Ctrl Pts',(-0.472397672264072,1.,-1.95296148278133));
#31787=CARTESIAN_POINT('Ctrl Pts',(-0.475848034683176,1.,-1.95796111148177));
#31788=CARTESIAN_POINT('Ctrl Pts',(-0.479349583074855,1.,-1.96294933055943));
#31789=CARTESIAN_POINT('Ctrl Pts',(-0.482901662120691,1.,-1.96792703422362));
#31790=CARTESIAN_POINT('Ctrl Pts',(-0.486502692907659,1.,-1.97289186263272));
#31791=CARTESIAN_POINT('Ctrl Pts',(-0.490150627860952,1.,-1.97783973019229));
#31792=CARTESIAN_POINT('Ctrl Pts',(-0.493843476541495,1.,-1.98276658761821));
#31793=CARTESIAN_POINT('Ctrl Pts',(-0.497579909545574,1.,-1.98767044752932));
#31794=CARTESIAN_POINT('Ctrl Pts',(-0.501359287727146,1.,-1.99255149126155));
#31795=CARTESIAN_POINT('Ctrl Pts',(-0.505181361323026,1.,-1.99741107463572));
#31796=CARTESIAN_POINT('Ctrl Pts',(-0.509046069886157,1.,-2.00225107134734));
#31797=CARTESIAN_POINT('Ctrl Pts',(-0.512953306961792,1.,-2.00707309946949));
#31798=CARTESIAN_POINT('Ctrl Pts',(-0.516902681728687,1.,-2.01187773939242));
#31799=CARTESIAN_POINT('Ctrl Pts',(-0.52089359039937,1.,-2.01666477917286));
#31800=CARTESIAN_POINT('Ctrl Pts',(-0.524925318333476,1.,-2.02143356304698));
#31801=CARTESIAN_POINT('Ctrl Pts',(-0.528997127241914,1.,-2.0261832908329));
#31802=CARTESIAN_POINT('Ctrl Pts',(-0.533108355132977,1.,-2.03091336214426));
#31803=CARTESIAN_POINT('Ctrl Pts',(-0.537258489833262,1.,-2.03562362954037));
#31804=CARTESIAN_POINT('Ctrl Pts',(-0.541447120615659,1.,-2.04031422690527));
#31805=CARTESIAN_POINT('Ctrl Pts',(-0.54567390381743,1.,-2.04498544714588));
#31806=CARTESIAN_POINT('Ctrl Pts',(-0.549938525150295,1.,-2.04963761077958));
#31807=CARTESIAN_POINT('Ctrl Pts',(-0.554240657463906,1.,-2.05427091604413));
#31808=CARTESIAN_POINT('Ctrl Pts',(-0.558579940185151,1.,-2.05888537756462));
#31809=CARTESIAN_POINT('Ctrl Pts',(-0.562955993082261,1.,-2.06348090160589));
#31810=CARTESIAN_POINT('Ctrl Pts',(-0.567368421181087,1.,-2.06805732997334));
#31811=CARTESIAN_POINT('Ctrl Pts',(-0.571816823242603,1.,-2.07261449292824));
#31812=CARTESIAN_POINT('Ctrl Pts',(-0.576300797416844,1.,-2.07715226767559));
#31813=CARTESIAN_POINT('Ctrl Pts',(-0.580819952108063,1.,-2.08167059018418));
#31814=CARTESIAN_POINT('Ctrl Pts',(-0.585373918991617,1.,-2.08616943727951));
#31815=CARTESIAN_POINT('Ctrl Pts',(-0.589962365403406,1.,-2.09064881812129));
#31816=CARTESIAN_POINT('Ctrl Pts',(-0.594585006052162,1.,-2.0951087622027));
#31817=CARTESIAN_POINT('Ctrl Pts',(-0.599241616420533,1.,-2.0995493086477));
#31818=CARTESIAN_POINT('Ctrl Pts',(-0.60393203073603,1.,-2.10397049886949));
#31819=CARTESIAN_POINT('Ctrl Pts',(-0.607711315454876,1.,-2.1074919961518));
#31820=CARTESIAN_POINT('Ctrl Pts',(-0.610560911689899,1.,-2.11012443807238));
#31821=CARTESIAN_POINT('Ctrl Pts',(-0.6124673655618,1.,-2.11187554259986));
#31822=CARTESIAN_POINT('Ctrl Pts',(-0.61342227326009,1.,-2.11275013067528));
#31823=CARTESIAN_POINT('',(-0.383122945602003,0.,-1.7075470150345));
#31824=CARTESIAN_POINT('Origin',(0.,0.,0.));
#31825=CARTESIAN_POINT('',(-0.163289472382896,1.,-1.74236521665491));
#31826=CARTESIAN_POINT('Origin',(0.,1.,0.));
#31827=CARTESIAN_POINT('',(-0.163289472382896,0.,-1.74236521665491));
#31828=CARTESIAN_POINT('Ctrl Pts',(-0.0694764450219581,-1.,-2.19890268624765));
#31829=CARTESIAN_POINT('Ctrl Pts',(-0.0694764450219581,1.,-2.19890268624765));
#31830=CARTESIAN_POINT('Ctrl Pts',(-0.070114353632549,-1.,-2.19777582085423));
#31831=CARTESIAN_POINT('Ctrl Pts',(-0.070114353632549,1.,-2.19777582085423));
#31832=CARTESIAN_POINT('Ctrl Pts',(-0.0713863779526154,-1.,-2.19552129484002));
#31833=CARTESIAN_POINT('Ctrl Pts',(-0.0713863779526154,1.,-2.19552129484002));
#31834=CARTESIAN_POINT('Ctrl Pts',(-0.0732830357306725,-1.,-2.19213712013662));
#31835=CARTESIAN_POINT('Ctrl Pts',(-0.0732830357306725,1.,-2.19213712013662));
#31836=CARTESIAN_POINT('Ctrl Pts',(-0.0757891465836148,-1.,-2.1876201139953));
#31837=CARTESIAN_POINT('Ctrl Pts',(-0.0757891465836148,1.,-2.1876201139953));
#31838=CARTESIAN_POINT('Ctrl Pts',(-0.0788837727685243,-1.,-2.18196589448887));
#31839=CARTESIAN_POINT('Ctrl Pts',(-0.0788837727685243,1.,-2.18196589448887));
#31840=CARTESIAN_POINT('Ctrl Pts',(-0.0819402680872765,-1.,-2.176303712113));
#31841=CARTESIAN_POINT('Ctrl Pts',(-0.0819402680872765,1.,-2.176303712113));
#31842=CARTESIAN_POINT('Ctrl Pts',(-0.0849584620835372,-1.,-2.17063357870952));
#31843=CARTESIAN_POINT('Ctrl Pts',(-0.0849584620835372,1.,-2.17063357870952));
#31844=CARTESIAN_POINT('Ctrl Pts',(-0.0879381291386923,-1.,-2.16495552645014));
#31845=CARTESIAN_POINT('Ctrl Pts',(-0.0879381291386923,1.,-2.16495552645014));
#31846=CARTESIAN_POINT('Ctrl Pts',(-0.0908789888107265,-1.,-2.15926961544516));
#31847=CARTESIAN_POINT('Ctrl Pts',(-0.0908789888107265,1.,-2.15926961544516));
#31848=CARTESIAN_POINT('Ctrl Pts',(-0.0937807218867643,-1.,-2.1535759397817));
#31849=CARTESIAN_POINT('Ctrl Pts',(-0.0937807218867643,1.,-2.1535759397817));
#31850=CARTESIAN_POINT('Ctrl Pts',(-0.0966429852305459,-1.,-2.14787463531795));
#31851=CARTESIAN_POINT('Ctrl Pts',(-0.0966429852305459,1.,-2.14787463531795));
#31852=CARTESIAN_POINT('Ctrl Pts',(-0.0994654261990915,-1.,-2.14216588396025));
#31853=CARTESIAN_POINT('Ctrl Pts',(-0.0994654261990915,1.,-2.14216588396025));
#31854=CARTESIAN_POINT('Ctrl Pts',(-0.1022477005561,-1.,-2.13644992667165));
#31855=CARTESIAN_POINT('Ctrl Pts',(-0.1022477005561,1.,-2.13644992667165));
#31856=CARTESIAN_POINT('Ctrl Pts',(-0.104989479152739,-1.,-2.13072704887293));
#31857=CARTESIAN_POINT('Ctrl Pts',(-0.104989479152739,1.,-2.13072704887293));
#31858=CARTESIAN_POINT('Ctrl Pts',(-0.10769043523109,-1.,-2.12499752307));
#31859=CARTESIAN_POINT('Ctrl Pts',(-0.10769043523109,1.,-2.12499752307));
#31860=CARTESIAN_POINT('Ctrl Pts',(-0.110350236135025,-1.,-2.11926155590865));
#31861=CARTESIAN_POINT('Ctrl Pts',(-0.110350236135025,1.,-2.11926155590865));
#31862=CARTESIAN_POINT('Ctrl Pts',(-0.112968534419737,-1.,-2.11351924490306));
#31863=CARTESIAN_POINT('Ctrl Pts',(-0.112968534419737,1.,-2.11351924490306));
#31864=CARTESIAN_POINT('Ctrl Pts',(-0.115544957687926,-1.,-2.10777050261309));
#31865=CARTESIAN_POINT('Ctrl Pts',(-0.115544957687926,1.,-2.10777050261309));
#31866=CARTESIAN_POINT('Ctrl Pts',(-0.118079107988355,-1.,-2.102015121329));
#31867=CARTESIAN_POINT('Ctrl Pts',(-0.118079107988355,1.,-2.102015121329));
#31868=CARTESIAN_POINT('Ctrl Pts',(-0.120570567965122,-1.,-2.0962529286773));
#31869=CARTESIAN_POINT('Ctrl Pts',(-0.120570567965122,1.,-2.0962529286773));
#31870=CARTESIAN_POINT('Ctrl Pts',(-0.123018905621083,-1.,-2.09048392424825));
#31871=CARTESIAN_POINT('Ctrl Pts',(-0.123018905621083,1.,-2.09048392424825));
#31872=CARTESIAN_POINT('Ctrl Pts',(-0.125423679412061,-1.,-2.08470840653643));
#31873=CARTESIAN_POINT('Ctrl Pts',(-0.125423679412061,1.,-2.08470840653643));
#31874=CARTESIAN_POINT('Ctrl Pts',(-0.12778444527612,-1.,-2.07892715110987));
#31875=CARTESIAN_POINT('Ctrl Pts',(-0.12778444527612,1.,-2.07892715110987));
#31876=CARTESIAN_POINT('Ctrl Pts',(-0.130100748328403,-1.,-2.07314114713063));
#31877=CARTESIAN_POINT('Ctrl Pts',(-0.130100748328403,1.,-2.07314114713063));
#31878=CARTESIAN_POINT('Ctrl Pts',(-0.13237211154771,-1.,-2.06735123910326));
#31879=CARTESIAN_POINT('Ctrl Pts',(-0.13237211154771,1.,-2.06735123910326));
#31880=CARTESIAN_POINT('Ctrl Pts',(-0.134598026192106,-1.,-2.06155781517842));
#31881=CARTESIAN_POINT('Ctrl Pts',(-0.134598026192106,1.,-2.06155781517842));
#31882=CARTESIAN_POINT('Ctrl Pts',(-0.136777941218044,-1.,-2.05576044414264));
#31883=CARTESIAN_POINT('Ctrl Pts',(-0.136777941218044,1.,-2.05576044414264));
#31884=CARTESIAN_POINT('Ctrl Pts',(-0.138911255368966,-1.,-2.04995762001328));
#31885=CARTESIAN_POINT('Ctrl Pts',(-0.138911255368966,1.,-2.04995762001328));
#31886=CARTESIAN_POINT('Ctrl Pts',(-0.140997332152546,-1.,-2.04414757947916));
#31887=CARTESIAN_POINT('Ctrl Pts',(-0.140997332152546,1.,-2.04414757947916));
#31888=CARTESIAN_POINT('Ctrl Pts',(-0.143035515058209,-1.,-2.03832911025912));
#31889=CARTESIAN_POINT('Ctrl Pts',(-0.143035515058209,1.,-2.03832911025912));
#31890=CARTESIAN_POINT('Ctrl Pts',(-0.145025140186057,-1.,-2.03250223739942));
#31891=CARTESIAN_POINT('Ctrl Pts',(-0.145025140186057,1.,-2.03250223739942));
#31892=CARTESIAN_POINT('Ctrl Pts',(-0.146965557332583,-1.,-2.02666926182017));
#31893=CARTESIAN_POINT('Ctrl Pts',(-0.146965557332583,1.,-2.02666926182017));
#31894=CARTESIAN_POINT('Ctrl Pts',(-0.148856124775337,-1.,-2.02083464969894));
#31895=CARTESIAN_POINT('Ctrl Pts',(-0.148856124775337,1.,-2.02083464969894));
#31896=CARTESIAN_POINT('Ctrl Pts',(-0.150696157673078,-1.,-2.01500291940238));
#31897=CARTESIAN_POINT('Ctrl Pts',(-0.150696157673078,1.,-2.01500291940238));
#31898=CARTESIAN_POINT('Ctrl Pts',(-0.15248488362145,-1.,-2.00917680318424));
#31899=CARTESIAN_POINT('Ctrl Pts',(-0.15248488362145,1.,-2.00917680318424));
#31900=CARTESIAN_POINT('Ctrl Pts',(-0.154221403049722,-1.,-2.00335565310543));
#31901=CARTESIAN_POINT('Ctrl Pts',(-0.154221403049722,1.,-2.00335565310543));
#31902=CARTESIAN_POINT('Ctrl Pts',(-0.155904629548783,-1.,-1.99753284771497));
#31903=CARTESIAN_POINT('Ctrl Pts',(-0.155904629548783,1.,-1.99753284771497));
#31904=CARTESIAN_POINT('Ctrl Pts',(-0.157533331459227,-1.,-1.99169810931908));
#31905=CARTESIAN_POINT('Ctrl Pts',(-0.157533331459227,1.,-1.99169810931908));
#31906=CARTESIAN_POINT('Ctrl Pts',(-0.159106226437299,-1.,-1.98584238283292));
#31907=CARTESIAN_POINT('Ctrl Pts',(-0.159106226437299,1.,-1.98584238283292));
#31908=CARTESIAN_POINT('Ctrl Pts',(-0.160622060784611,-1.,-1.97996195437559));
#31909=CARTESIAN_POINT('Ctrl Pts',(-0.160622060784611,1.,-1.97996195437559));
#31910=CARTESIAN_POINT('Ctrl Pts',(-0.162079693556289,-1.,-1.97406280235188));
#31911=CARTESIAN_POINT('Ctrl Pts',(-0.162079693556289,1.,-1.97406280235188));
#31912=CARTESIAN_POINT('Ctrl Pts',(-0.163478185457734,-1.,-1.96816512677967));
#31913=CARTESIAN_POINT('Ctrl Pts',(-0.163478185457734,1.,-1.96816512677967));
#31914=CARTESIAN_POINT('Ctrl Pts',(-0.164816568920269,-1.,-1.96229379940136));
#31915=CARTESIAN_POINT('Ctrl Pts',(-0.164816568920269,1.,-1.96229379940136));
#31916=CARTESIAN_POINT('Ctrl Pts',(-0.166093592002812,-1.,-1.9564675971873));
#31917=CARTESIAN_POINT('Ctrl Pts',(-0.166093592002812,1.,-1.9564675971873));
#31918=CARTESIAN_POINT('Ctrl Pts',(-0.167307501784475,-1.,-1.95069027794294));
#31919=CARTESIAN_POINT('Ctrl Pts',(-0.167307501784475,1.,-1.95069027794294));
#31920=CARTESIAN_POINT('Ctrl Pts',(-0.168455741607556,-1.,-1.94493757756931));
#31921=CARTESIAN_POINT('Ctrl Pts',(-0.168455741607556,1.,-1.94493757756931));
#31922=CARTESIAN_POINT('Ctrl Pts',(-0.169534904817491,-1.,-1.93915639211581));
#31923=CARTESIAN_POINT('Ctrl Pts',(-0.169534904817491,1.,-1.93915639211581));
#31924=CARTESIAN_POINT('Ctrl Pts',(-0.170541253116202,-1.,-1.93329183155539));
#31925=CARTESIAN_POINT('Ctrl Pts',(-0.170541253116202,1.,-1.93329183155539));
#31926=CARTESIAN_POINT('Ctrl Pts',(-0.171471191532988,-1.,-1.92731093582036));
#31927=CARTESIAN_POINT('Ctrl Pts',(-0.171471191532988,1.,-1.92731093582036));
#31928=CARTESIAN_POINT('Ctrl Pts',(-0.172321621259514,-1.,-1.9212233439798));
#31929=CARTESIAN_POINT('Ctrl Pts',(-0.172321621259514,1.,-1.9212233439798));
#31930=CARTESIAN_POINT('Ctrl Pts',(-0.173090695383496,-1.,-1.91511429159527));
#31931=CARTESIAN_POINT('Ctrl Pts',(-0.173090695383496,1.,-1.91511429159527));
#31932=CARTESIAN_POINT('Ctrl Pts',(-0.173776635257817,-1.,-1.90911693975267));
#31933=CARTESIAN_POINT('Ctrl Pts',(-0.173776635257817,1.,-1.90911693975267));
#31934=CARTESIAN_POINT('Ctrl Pts',(-0.174375518661085,-1.,-1.90335253862834));
#31935=CARTESIAN_POINT('Ctrl Pts',(-0.174375518661085,1.,-1.90335253862834));
#31936=CARTESIAN_POINT('Ctrl Pts',(-0.174879405091263,-1.,-1.89788101117132));
#31937=CARTESIAN_POINT('Ctrl Pts',(-0.174879405091263,1.,-1.89788101117132));
#31938=CARTESIAN_POINT('Ctrl Pts',(-0.175274276190844,-1.,-1.892646301985));
#31939=CARTESIAN_POINT('Ctrl Pts',(-0.175274276190844,1.,-1.892646301985));
#31940=CARTESIAN_POINT('Ctrl Pts',(-0.175538155840648,-1.,-1.88742606273259));
#31941=CARTESIAN_POINT('Ctrl Pts',(-0.175538155840648,1.,-1.88742606273259));
#31942=CARTESIAN_POINT('Ctrl Pts',(-0.175644148889699,-1.,-1.88188663145367));
#31943=CARTESIAN_POINT('Ctrl Pts',(-0.175644148889699,1.,-1.88188663145367));
#31944=CARTESIAN_POINT('Ctrl Pts',(-0.175563480746485,-1.,-1.87563767773588));
#31945=CARTESIAN_POINT('Ctrl Pts',(-0.175563480746485,1.,-1.87563767773588));
#31946=CARTESIAN_POINT('Ctrl Pts',(-0.175268337590758,-1.,-1.86828349694799));
#31947=CARTESIAN_POINT('Ctrl Pts',(-0.175268337590758,1.,-1.86828349694799));
#31948=CARTESIAN_POINT('Ctrl Pts',(-0.17473525927603,-1.,-1.85948367088837));
#31949=CARTESIAN_POINT('Ctrl Pts',(-0.17473525927603,1.,-1.85948367088837));
#31950=CARTESIAN_POINT('Ctrl Pts',(-0.173946627587731,-1.,-1.8489811319852));
#31951=CARTESIAN_POINT('Ctrl Pts',(-0.173946627587731,1.,-1.8489811319852));
#31952=CARTESIAN_POINT('Ctrl Pts',(-0.1728894428919,-1.,-1.83658380527692));
#31953=CARTESIAN_POINT('Ctrl Pts',(-0.1728894428919,1.,-1.83658380527692));
#31954=CARTESIAN_POINT('Ctrl Pts',(-0.171554770204119,-1.,-1.82215766811545));
#31955=CARTESIAN_POINT('Ctrl Pts',(-0.171554770204119,1.,-1.82215766811545));
#31956=CARTESIAN_POINT('Ctrl Pts',(-0.169936923904608,-1.,-1.80561530629706));
#31957=CARTESIAN_POINT('Ctrl Pts',(-0.169936923904608,1.,-1.80561530629706));
#31958=CARTESIAN_POINT('Ctrl Pts',(-0.168032772805197,-1.,-1.7869064998507));
#31959=CARTESIAN_POINT('Ctrl Pts',(-0.168032772805197,1.,-1.7869064998507));
#31960=CARTESIAN_POINT('Ctrl Pts',(-0.1662793551464,-1.,-1.77018771684844));
#31961=CARTESIAN_POINT('Ctrl Pts',(-0.1662793551464,1.,-1.77018771684844));
#31962=CARTESIAN_POINT('Ctrl Pts',(-0.164834765707158,-1.,-1.75666056638427));
#31963=CARTESIAN_POINT('Ctrl Pts',(-0.164834765707158,1.,-1.75666056638427));
#31964=CARTESIAN_POINT('Ctrl Pts',(-0.163814161002002,-1.,-1.7472034950333));
#31965=CARTESIAN_POINT('Ctrl Pts',(-0.163814161002002,1.,-1.7472034950333));
#31966=CARTESIAN_POINT('Ctrl Pts',(-0.163289472382896,-1.,-1.74236521665491));
#31967=CARTESIAN_POINT('Ctrl Pts',(-0.163289472382896,1.,-1.74236521665491));
#31968=CARTESIAN_POINT('',(-0.0694764450219581,1.,-2.19890268624765));
#31969=CARTESIAN_POINT('Ctrl Pts',(-0.0694764450219581,1.,-2.19890268624765));
#31970=CARTESIAN_POINT('Ctrl Pts',(-0.070114353632549,1.,-2.19777582085423));
#31971=CARTESIAN_POINT('Ctrl Pts',(-0.0713863779526154,1.,-2.19552129484002));
#31972=CARTESIAN_POINT('Ctrl Pts',(-0.0732830357306725,1.,-2.19213712013662));
#31973=CARTESIAN_POINT('Ctrl Pts',(-0.0757891465836148,1.,-2.1876201139953));
#31974=CARTESIAN_POINT('Ctrl Pts',(-0.0788837727685243,1.,-2.18196589448887));
#31975=CARTESIAN_POINT('Ctrl Pts',(-0.0819402680872765,1.,-2.176303712113));
#31976=CARTESIAN_POINT('Ctrl Pts',(-0.0849584620835372,1.,-2.17063357870952));
#31977=CARTESIAN_POINT('Ctrl Pts',(-0.0879381291386923,1.,-2.16495552645014));
#31978=CARTESIAN_POINT('Ctrl Pts',(-0.0908789888107265,1.,-2.15926961544516));
#31979=CARTESIAN_POINT('Ctrl Pts',(-0.0937807218867643,1.,-2.1535759397817));
#31980=CARTESIAN_POINT('Ctrl Pts',(-0.0966429852305459,1.,-2.14787463531795));
#31981=CARTESIAN_POINT('Ctrl Pts',(-0.0994654261990915,1.,-2.14216588396025));
#31982=CARTESIAN_POINT('Ctrl Pts',(-0.1022477005561,1.,-2.13644992667165));
#31983=CARTESIAN_POINT('Ctrl Pts',(-0.104989479152739,1.,-2.13072704887293));
#31984=CARTESIAN_POINT('Ctrl Pts',(-0.10769043523109,1.,-2.12499752307));
#31985=CARTESIAN_POINT('Ctrl Pts',(-0.110350236135025,1.,-2.11926155590865));
#31986=CARTESIAN_POINT('Ctrl Pts',(-0.112968534419737,1.,-2.11351924490306));
#31987=CARTESIAN_POINT('Ctrl Pts',(-0.115544957687926,1.,-2.10777050261309));
#31988=CARTESIAN_POINT('Ctrl Pts',(-0.118079107988355,1.,-2.102015121329));
#31989=CARTESIAN_POINT('Ctrl Pts',(-0.120570567965122,1.,-2.0962529286773));
#31990=CARTESIAN_POINT('Ctrl Pts',(-0.123018905621083,1.,-2.09048392424825));
#31991=CARTESIAN_POINT('Ctrl Pts',(-0.125423679412061,1.,-2.08470840653643));
#31992=CARTESIAN_POINT('Ctrl Pts',(-0.12778444527612,1.,-2.07892715110987));
#31993=CARTESIAN_POINT('Ctrl Pts',(-0.130100748328403,1.,-2.07314114713063));
#31994=CARTESIAN_POINT('Ctrl Pts',(-0.13237211154771,1.,-2.06735123910326));
#31995=CARTESIAN_POINT('Ctrl Pts',(-0.134598026192106,1.,-2.06155781517842));
#31996=CARTESIAN_POINT('Ctrl Pts',(-0.136777941218044,1.,-2.05576044414264));
#31997=CARTESIAN_POINT('Ctrl Pts',(-0.138911255368966,1.,-2.04995762001328));
#31998=CARTESIAN_POINT('Ctrl Pts',(-0.140997332152546,1.,-2.04414757947916));
#31999=CARTESIAN_POINT('Ctrl Pts',(-0.143035515058209,1.,-2.03832911025912));
#32000=CARTESIAN_POINT('Ctrl Pts',(-0.145025140186057,1.,-2.03250223739942));
#32001=CARTESIAN_POINT('Ctrl Pts',(-0.146965557332583,1.,-2.02666926182017));
#32002=CARTESIAN_POINT('Ctrl Pts',(-0.148856124775337,1.,-2.02083464969894));
#32003=CARTESIAN_POINT('Ctrl Pts',(-0.150696157673078,1.,-2.01500291940238));
#32004=CARTESIAN_POINT('Ctrl Pts',(-0.15248488362145,1.,-2.00917680318424));
#32005=CARTESIAN_POINT('Ctrl Pts',(-0.154221403049722,1.,-2.00335565310543));
#32006=CARTESIAN_POINT('Ctrl Pts',(-0.155904629548783,1.,-1.99753284771497));
#32007=CARTESIAN_POINT('Ctrl Pts',(-0.157533331459227,1.,-1.99169810931908));
#32008=CARTESIAN_POINT('Ctrl Pts',(-0.159106226437299,1.,-1.98584238283292));
#32009=CARTESIAN_POINT('Ctrl Pts',(-0.160622060784611,1.,-1.97996195437559));
#32010=CARTESIAN_POINT('Ctrl Pts',(-0.162079693556289,1.,-1.97406280235188));
#32011=CARTESIAN_POINT('Ctrl Pts',(-0.163478185457734,1.,-1.96816512677967));
#32012=CARTESIAN_POINT('Ctrl Pts',(-0.164816568920269,1.,-1.96229379940136));
#32013=CARTESIAN_POINT('Ctrl Pts',(-0.166093592002812,1.,-1.9564675971873));
#32014=CARTESIAN_POINT('Ctrl Pts',(-0.167307501784475,1.,-1.95069027794294));
#32015=CARTESIAN_POINT('Ctrl Pts',(-0.168455741607556,1.,-1.94493757756931));
#32016=CARTESIAN_POINT('Ctrl Pts',(-0.169534904817491,1.,-1.93915639211581));
#32017=CARTESIAN_POINT('Ctrl Pts',(-0.170541253116202,1.,-1.93329183155539));
#32018=CARTESIAN_POINT('Ctrl Pts',(-0.171471191532988,1.,-1.92731093582036));
#32019=CARTESIAN_POINT('Ctrl Pts',(-0.172321621259514,1.,-1.9212233439798));
#32020=CARTESIAN_POINT('Ctrl Pts',(-0.173090695383496,1.,-1.91511429159527));
#32021=CARTESIAN_POINT('Ctrl Pts',(-0.173776635257817,1.,-1.90911693975267));
#32022=CARTESIAN_POINT('Ctrl Pts',(-0.174375518661085,1.,-1.90335253862834));
#32023=CARTESIAN_POINT('Ctrl Pts',(-0.174879405091263,1.,-1.89788101117132));
#32024=CARTESIAN_POINT('Ctrl Pts',(-0.175274276190844,1.,-1.892646301985));
#32025=CARTESIAN_POINT('Ctrl Pts',(-0.175538155840648,1.,-1.88742606273259));
#32026=CARTESIAN_POINT('Ctrl Pts',(-0.175644148889699,1.,-1.88188663145367));
#32027=CARTESIAN_POINT('Ctrl Pts',(-0.175563480746485,1.,-1.87563767773588));
#32028=CARTESIAN_POINT('Ctrl Pts',(-0.175268337590758,1.,-1.86828349694799));
#32029=CARTESIAN_POINT('Ctrl Pts',(-0.17473525927603,1.,-1.85948367088837));
#32030=CARTESIAN_POINT('Ctrl Pts',(-0.173946627587731,1.,-1.8489811319852));
#32031=CARTESIAN_POINT('Ctrl Pts',(-0.1728894428919,1.,-1.83658380527692));
#32032=CARTESIAN_POINT('Ctrl Pts',(-0.171554770204119,1.,-1.82215766811545));
#32033=CARTESIAN_POINT('Ctrl Pts',(-0.169936923904608,1.,-1.80561530629706));
#32034=CARTESIAN_POINT('Ctrl Pts',(-0.168032772805197,1.,-1.7869064998507));
#32035=CARTESIAN_POINT('Ctrl Pts',(-0.1662793551464,1.,-1.77018771684844));
#32036=CARTESIAN_POINT('Ctrl Pts',(-0.164834765707158,1.,-1.75666056638427));
#32037=CARTESIAN_POINT('Ctrl Pts',(-0.163814161002002,1.,-1.7472034950333));
#32038=CARTESIAN_POINT('Ctrl Pts',(-0.163289472382896,1.,-1.74236521665491));
#32039=CARTESIAN_POINT('',(-0.0694764450219581,0.,-2.19890268624765));
#32040=CARTESIAN_POINT('Origin',(0.0694764450219584,0.,-2.19890268624765));
#32041=CARTESIAN_POINT('',(0.0694764450219584,1.,-2.19890268624765));
#32042=CARTESIAN_POINT('',(-0.0694764450219581,1.,-2.19890268624765));
#32043=CARTESIAN_POINT('',(0.0694764450219584,0.,-2.19890268624765));
#32044=CARTESIAN_POINT('Ctrl Pts',(0.163289472382896,-1.,-1.74236521665491));
#32045=CARTESIAN_POINT('Ctrl Pts',(0.163289472382896,1.,-1.74236521665491));
#32046=CARTESIAN_POINT('Ctrl Pts',(0.163814161002474,-1.,-1.74720349503904));
#32047=CARTESIAN_POINT('Ctrl Pts',(0.163814161002474,1.,-1.74720349503904));
#32048=CARTESIAN_POINT('Ctrl Pts',(0.164834765708484,-1.,-1.75666056640041));
#32049=CARTESIAN_POINT('Ctrl Pts',(0.164834765708484,1.,-1.75666056640041));
#32050=CARTESIAN_POINT('Ctrl Pts',(0.166279355148738,-1.,-1.77018771687692));
#32051=CARTESIAN_POINT('Ctrl Pts',(0.166279355148738,1.,-1.77018771687692));
#32052=CARTESIAN_POINT('Ctrl Pts',(0.16803277280837,-1.,-1.78690649988931));
#32053=CARTESIAN_POINT('Ctrl Pts',(0.16803277280837,1.,-1.78690649988931));
#32054=CARTESIAN_POINT('Ctrl Pts',(0.169936923908078,-1.,-1.80561530633924));
#32055=CARTESIAN_POINT('Ctrl Pts',(0.169936923908078,1.,-1.80561530633924));
#32056=CARTESIAN_POINT('Ctrl Pts',(0.171554770207306,-1.,-1.82215766815414));
#32057=CARTESIAN_POINT('Ctrl Pts',(0.171554770207306,1.,-1.82215766815414));
#32058=CARTESIAN_POINT('Ctrl Pts',(0.17288944289442,-1.,-1.83658380530747));
#32059=CARTESIAN_POINT('Ctrl Pts',(0.17288944289442,1.,-1.83658380530747));
#32060=CARTESIAN_POINT('Ctrl Pts',(0.173946627589401,-1.,-1.84898113200543));
#32061=CARTESIAN_POINT('Ctrl Pts',(0.173946627589401,1.,-1.84898113200543));
#32062=CARTESIAN_POINT('Ctrl Pts',(0.174735259276856,-1.,-1.85948367089838));
#32063=CARTESIAN_POINT('Ctrl Pts',(0.174735259276856,1.,-1.85948367089838));
#32064=CARTESIAN_POINT('Ctrl Pts',(0.175268337590901,-1.,-1.86828349694972));
#32065=CARTESIAN_POINT('Ctrl Pts',(0.175268337590901,1.,-1.86828349694972));
#32066=CARTESIAN_POINT('Ctrl Pts',(0.175563480746205,-1.,-1.87563767773249));
#32067=CARTESIAN_POINT('Ctrl Pts',(0.175563480746205,1.,-1.87563767773249));
#32068=CARTESIAN_POINT('Ctrl Pts',(0.175644148889271,-1.,-1.88188663144846));
#32069=CARTESIAN_POINT('Ctrl Pts',(0.175644148889271,1.,-1.88188663144846));
#32070=CARTESIAN_POINT('Ctrl Pts',(0.175538155840286,-1.,-1.88742606272818));
#32071=CARTESIAN_POINT('Ctrl Pts',(0.175538155840286,1.,-1.88742606272818));
#32072=CARTESIAN_POINT('Ctrl Pts',(0.175274276190664,-1.,-1.89264630198279));
#32073=CARTESIAN_POINT('Ctrl Pts',(0.175274276190664,1.,-1.89264630198279));
#32074=CARTESIAN_POINT('Ctrl Pts',(0.174879405091277,-1.,-1.89788101117148));
#32075=CARTESIAN_POINT('Ctrl Pts',(0.174879405091277,1.,-1.89788101117148));
#32076=CARTESIAN_POINT('Ctrl Pts',(0.174375518661222,-1.,-1.90335253863003));
#32077=CARTESIAN_POINT('Ctrl Pts',(0.174375518661222,1.,-1.90335253863003));
#32078=CARTESIAN_POINT('Ctrl Pts',(0.173776635257984,-1.,-1.90911693975475));
#32079=CARTESIAN_POINT('Ctrl Pts',(0.173776635257984,1.,-1.90911693975475));
#32080=CARTESIAN_POINT('Ctrl Pts',(0.173090695383619,-1.,-1.91511429159681));
#32081=CARTESIAN_POINT('Ctrl Pts',(0.173090695383619,1.,-1.91511429159681));
#32082=CARTESIAN_POINT('Ctrl Pts',(0.172321621259557,-1.,-1.92122334398034));
#32083=CARTESIAN_POINT('Ctrl Pts',(0.172321621259557,1.,-1.92122334398034));
#32084=CARTESIAN_POINT('Ctrl Pts',(0.17147119153296,-1.,-1.92731093582));
#32085=CARTESIAN_POINT('Ctrl Pts',(0.17147119153296,1.,-1.92731093582));
#32086=CARTESIAN_POINT('Ctrl Pts',(0.170541253116136,-1.,-1.93329183155455));
#32087=CARTESIAN_POINT('Ctrl Pts',(0.170541253116136,1.,-1.93329183155455));
#32088=CARTESIAN_POINT('Ctrl Pts',(0.169534904817425,-1.,-1.93915639211497));
#32089=CARTESIAN_POINT('Ctrl Pts',(0.169534904817425,1.,-1.93915639211497));
#32090=CARTESIAN_POINT('Ctrl Pts',(0.168455741607516,-1.,-1.94493757756879));
#32091=CARTESIAN_POINT('Ctrl Pts',(0.168455741607516,1.,-1.94493757756879));
#32092=CARTESIAN_POINT('Ctrl Pts',(0.167307501784469,-1.,-1.95069027794286));
#32093=CARTESIAN_POINT('Ctrl Pts',(0.167307501784469,1.,-1.95069027794286));
#32094=CARTESIAN_POINT('Ctrl Pts',(0.166093592002833,-1.,-1.95646759718755));
#32095=CARTESIAN_POINT('Ctrl Pts',(0.166093592002833,1.,-1.95646759718755));
#32096=CARTESIAN_POINT('Ctrl Pts',(0.1648165689203,-1.,-1.96229379940174));
#32097=CARTESIAN_POINT('Ctrl Pts',(0.1648165689203,1.,-1.96229379940174));
#32098=CARTESIAN_POINT('Ctrl Pts',(0.16347818545776,-1.,-1.96816512678));
#32099=CARTESIAN_POINT('Ctrl Pts',(0.16347818545776,1.,-1.96816512678));
#32100=CARTESIAN_POINT('Ctrl Pts',(0.162079693556302,-1.,-1.97406280235204));
#32101=CARTESIAN_POINT('Ctrl Pts',(0.162079693556302,1.,-1.97406280235204));
#32102=CARTESIAN_POINT('Ctrl Pts',(0.16062206078461,-1.,-1.97996195437557));
#32103=CARTESIAN_POINT('Ctrl Pts',(0.16062206078461,1.,-1.97996195437557));
#32104=CARTESIAN_POINT('Ctrl Pts',(0.159106226437288,-1.,-1.98584238283279));
#32105=CARTESIAN_POINT('Ctrl Pts',(0.159106226437288,1.,-1.98584238283279));
#32106=CARTESIAN_POINT('Ctrl Pts',(0.157533331459215,-1.,-1.99169810931893));
#32107=CARTESIAN_POINT('Ctrl Pts',(0.157533331459215,1.,-1.99169810931893));
#32108=CARTESIAN_POINT('Ctrl Pts',(0.155904629548774,-1.,-1.99753284771487));
#32109=CARTESIAN_POINT('Ctrl Pts',(0.155904629548774,1.,-1.99753284771487));
#32110=CARTESIAN_POINT('Ctrl Pts',(0.154221403049719,-1.,-2.00335565310539));
#32111=CARTESIAN_POINT('Ctrl Pts',(0.154221403049719,1.,-2.00335565310539));
#32112=CARTESIAN_POINT('Ctrl Pts',(0.152484883621452,-1.,-2.00917680318426));
#32113=CARTESIAN_POINT('Ctrl Pts',(0.152484883621452,1.,-2.00917680318426));
#32114=CARTESIAN_POINT('Ctrl Pts',(0.150696157673084,-1.,-2.01500291940243));
#32115=CARTESIAN_POINT('Ctrl Pts',(0.150696157673084,1.,-2.01500291940243));
#32116=CARTESIAN_POINT('Ctrl Pts',(0.148856124775343,-1.,-2.02083464969897));
#32117=CARTESIAN_POINT('Ctrl Pts',(0.148856124775343,1.,-2.02083464969897));
#32118=CARTESIAN_POINT('Ctrl Pts',(0.146965557332586,-1.,-2.02666926182017));
#32119=CARTESIAN_POINT('Ctrl Pts',(0.146965557332586,1.,-2.02666926182017));
#32120=CARTESIAN_POINT('Ctrl Pts',(0.145025140186058,-1.,-2.03250223739941));
#32121=CARTESIAN_POINT('Ctrl Pts',(0.145025140186058,1.,-2.03250223739941));
#32122=CARTESIAN_POINT('Ctrl Pts',(0.143035515058208,-1.,-2.03832911025913));
#32123=CARTESIAN_POINT('Ctrl Pts',(0.143035515058208,1.,-2.03832911025913));
#32124=CARTESIAN_POINT('Ctrl Pts',(0.140997332152545,-1.,-2.04414757947919));
#32125=CARTESIAN_POINT('Ctrl Pts',(0.140997332152545,1.,-2.04414757947919));
#32126=CARTESIAN_POINT('Ctrl Pts',(0.138911255368966,-1.,-2.04995762001333));
#32127=CARTESIAN_POINT('Ctrl Pts',(0.138911255368966,1.,-2.04995762001333));
#32128=CARTESIAN_POINT('Ctrl Pts',(0.136777941218044,-1.,-2.0557604441427));
#32129=CARTESIAN_POINT('Ctrl Pts',(0.136777941218044,1.,-2.0557604441427));
#32130=CARTESIAN_POINT('Ctrl Pts',(0.134598026192107,-1.,-2.06155781517844));
#32131=CARTESIAN_POINT('Ctrl Pts',(0.134598026192107,1.,-2.06155781517844));
#32132=CARTESIAN_POINT('Ctrl Pts',(0.13237211154771,-1.,-2.06735123910319));
#32133=CARTESIAN_POINT('Ctrl Pts',(0.13237211154771,1.,-2.06735123910319));
#32134=CARTESIAN_POINT('Ctrl Pts',(0.1301007483284,-1.,-2.07314114713047));
#32135=CARTESIAN_POINT('Ctrl Pts',(0.1301007483284,1.,-2.07314114713047));
#32136=CARTESIAN_POINT('Ctrl Pts',(0.127784445276116,-1.,-2.07892715110967));
#32137=CARTESIAN_POINT('Ctrl Pts',(0.127784445276116,1.,-2.07892715110967));
#32138=CARTESIAN_POINT('Ctrl Pts',(0.125423679412058,-1.,-2.08470840653628));
#32139=CARTESIAN_POINT('Ctrl Pts',(0.125423679412058,1.,-2.08470840653628));
#32140=CARTESIAN_POINT('Ctrl Pts',(0.123018905621083,-1.,-2.09048392424826));
#32141=CARTESIAN_POINT('Ctrl Pts',(0.123018905621083,1.,-2.09048392424826));
#32142=CARTESIAN_POINT('Ctrl Pts',(0.120570567965129,-1.,-2.09625292867756));
#32143=CARTESIAN_POINT('Ctrl Pts',(0.120570567965129,1.,-2.09625292867756));
#32144=CARTESIAN_POINT('Ctrl Pts',(0.118079107988368,-1.,-2.10201512132945));
#32145=CARTESIAN_POINT('Ctrl Pts',(0.118079107988368,1.,-2.10201512132945));
#32146=CARTESIAN_POINT('Ctrl Pts',(0.11554495768794,-1.,-2.10777050261359));
#32147=CARTESIAN_POINT('Ctrl Pts',(0.11554495768794,1.,-2.10777050261359));
#32148=CARTESIAN_POINT('Ctrl Pts',(0.112968534419746,-1.,-2.11351924490335));
#32149=CARTESIAN_POINT('Ctrl Pts',(0.112968534419746,1.,-2.11351924490335));
#32150=CARTESIAN_POINT('Ctrl Pts',(0.11035023613502,-1.,-2.11926155590849));
#32151=CARTESIAN_POINT('Ctrl Pts',(0.11035023613502,1.,-2.11926155590849));
#32152=CARTESIAN_POINT('Ctrl Pts',(0.107690435231068,-1.,-2.12499752306927));
#32153=CARTESIAN_POINT('Ctrl Pts',(0.107690435231068,1.,-2.12499752306927));
#32154=CARTESIAN_POINT('Ctrl Pts',(0.104989479152703,-1.,-2.1307270488718));
#32155=CARTESIAN_POINT('Ctrl Pts',(0.104989479152703,1.,-2.1307270488718));
#32156=CARTESIAN_POINT('Ctrl Pts',(0.102247700556064,-1.,-2.13644992667052));
#32157=CARTESIAN_POINT('Ctrl Pts',(0.102247700556064,1.,-2.13644992667052));
#32158=CARTESIAN_POINT('Ctrl Pts',(0.0994654261990743,-1.,-2.14216588395974));
#32159=CARTESIAN_POINT('Ctrl Pts',(0.0994654261990743,1.,-2.14216588395974));
#32160=CARTESIAN_POINT('Ctrl Pts',(0.0966429852305689,-1.,-2.14787463531864));
#32161=CARTESIAN_POINT('Ctrl Pts',(0.0966429852305689,1.,-2.14787463531864));
#32162=CARTESIAN_POINT('Ctrl Pts',(0.0937807218868345,-1.,-2.15357593978377));
#32163=CARTESIAN_POINT('Ctrl Pts',(0.0937807218868345,1.,-2.15357593978377));
#32164=CARTESIAN_POINT('Ctrl Pts',(0.0908789888108266,-1.,-2.15926961544808));
#32165=CARTESIAN_POINT('Ctrl Pts',(0.0908789888108266,1.,-2.15926961544808));
#32166=CARTESIAN_POINT('Ctrl Pts',(0.0879381291387823,-1.,-2.16495552645275));
#32167=CARTESIAN_POINT('Ctrl Pts',(0.0879381291387823,1.,-2.16495552645275));
#32168=CARTESIAN_POINT('Ctrl Pts',(0.0849584620835643,-1.,-2.17063357871031));
#32169=CARTESIAN_POINT('Ctrl Pts',(0.0849584620835643,1.,-2.17063357871031));
#32170=CARTESIAN_POINT('Ctrl Pts',(0.0819402680871939,-1.,-2.1763037121106));
#32171=CARTESIAN_POINT('Ctrl Pts',(0.0819402680871939,1.,-2.1763037121106));
#32172=CARTESIAN_POINT('Ctrl Pts',(0.0788837727683228,-1.,-2.18196589448304));
#32173=CARTESIAN_POINT('Ctrl Pts',(0.0788837727683228,1.,-2.18196589448304));
#32174=CARTESIAN_POINT('Ctrl Pts',(0.0757891465833411,-1.,-2.1876201139874));
#32175=CARTESIAN_POINT('Ctrl Pts',(0.0757891465833411,1.,-2.1876201139874));
#32176=CARTESIAN_POINT('Ctrl Pts',(0.0732830357304276,-1.,-2.19213712012956));
#32177=CARTESIAN_POINT('Ctrl Pts',(0.0732830357304276,1.,-2.19213712012956));
#32178=CARTESIAN_POINT('Ctrl Pts',(0.0713863779524627,-1.,-2.19552129483562));
#32179=CARTESIAN_POINT('Ctrl Pts',(0.0713863779524627,1.,-2.19552129483562));
#32180=CARTESIAN_POINT('Ctrl Pts',(0.0701143536324926,-1.,-2.19777582085261));
#32181=CARTESIAN_POINT('Ctrl Pts',(0.0701143536324926,1.,-2.19777582085261));
#32182=CARTESIAN_POINT('Ctrl Pts',(0.0694764450219584,-1.,-2.19890268624765));
#32183=CARTESIAN_POINT('Ctrl Pts',(0.0694764450219584,1.,-2.19890268624765));
#32184=CARTESIAN_POINT('',(0.163289472382896,1.,-1.74236521665491));
#32185=CARTESIAN_POINT('Ctrl Pts',(0.163289472382896,1.,-1.74236521665491));
#32186=CARTESIAN_POINT('Ctrl Pts',(0.163814161002474,1.,-1.74720349503904));
#32187=CARTESIAN_POINT('Ctrl Pts',(0.164834765708484,1.,-1.75666056640041));
#32188=CARTESIAN_POINT('Ctrl Pts',(0.166279355148738,1.,-1.77018771687692));
#32189=CARTESIAN_POINT('Ctrl Pts',(0.16803277280837,1.,-1.78690649988931));
#32190=CARTESIAN_POINT('Ctrl Pts',(0.169936923908078,1.,-1.80561530633924));
#32191=CARTESIAN_POINT('Ctrl Pts',(0.171554770207306,1.,-1.82215766815414));
#32192=CARTESIAN_POINT('Ctrl Pts',(0.17288944289442,1.,-1.83658380530747));
#32193=CARTESIAN_POINT('Ctrl Pts',(0.173946627589401,1.,-1.84898113200543));
#32194=CARTESIAN_POINT('Ctrl Pts',(0.174735259276856,1.,-1.85948367089838));
#32195=CARTESIAN_POINT('Ctrl Pts',(0.175268337590901,1.,-1.86828349694972));
#32196=CARTESIAN_POINT('Ctrl Pts',(0.175563480746205,1.,-1.87563767773249));
#32197=CARTESIAN_POINT('Ctrl Pts',(0.175644148889271,1.,-1.88188663144846));
#32198=CARTESIAN_POINT('Ctrl Pts',(0.175538155840286,1.,-1.88742606272818));
#32199=CARTESIAN_POINT('Ctrl Pts',(0.175274276190664,1.,-1.89264630198279));
#32200=CARTESIAN_POINT('Ctrl Pts',(0.174879405091277,1.,-1.89788101117148));
#32201=CARTESIAN_POINT('Ctrl Pts',(0.174375518661222,1.,-1.90335253863003));
#32202=CARTESIAN_POINT('Ctrl Pts',(0.173776635257984,1.,-1.90911693975475));
#32203=CARTESIAN_POINT('Ctrl Pts',(0.173090695383619,1.,-1.91511429159681));
#32204=CARTESIAN_POINT('Ctrl Pts',(0.172321621259557,1.,-1.92122334398034));
#32205=CARTESIAN_POINT('Ctrl Pts',(0.17147119153296,1.,-1.92731093582));
#32206=CARTESIAN_POINT('Ctrl Pts',(0.170541253116136,1.,-1.93329183155455));
#32207=CARTESIAN_POINT('Ctrl Pts',(0.169534904817425,1.,-1.93915639211497));
#32208=CARTESIAN_POINT('Ctrl Pts',(0.168455741607516,1.,-1.94493757756879));
#32209=CARTESIAN_POINT('Ctrl Pts',(0.167307501784469,1.,-1.95069027794286));
#32210=CARTESIAN_POINT('Ctrl Pts',(0.166093592002833,1.,-1.95646759718755));
#32211=CARTESIAN_POINT('Ctrl Pts',(0.1648165689203,1.,-1.96229379940174));
#32212=CARTESIAN_POINT('Ctrl Pts',(0.16347818545776,1.,-1.96816512678));
#32213=CARTESIAN_POINT('Ctrl Pts',(0.162079693556302,1.,-1.97406280235204));
#32214=CARTESIAN_POINT('Ctrl Pts',(0.16062206078461,1.,-1.97996195437557));
#32215=CARTESIAN_POINT('Ctrl Pts',(0.159106226437288,1.,-1.98584238283279));
#32216=CARTESIAN_POINT('Ctrl Pts',(0.157533331459215,1.,-1.99169810931893));
#32217=CARTESIAN_POINT('Ctrl Pts',(0.155904629548774,1.,-1.99753284771487));
#32218=CARTESIAN_POINT('Ctrl Pts',(0.154221403049719,1.,-2.00335565310539));
#32219=CARTESIAN_POINT('Ctrl Pts',(0.152484883621452,1.,-2.00917680318426));
#32220=CARTESIAN_POINT('Ctrl Pts',(0.150696157673084,1.,-2.01500291940243));
#32221=CARTESIAN_POINT('Ctrl Pts',(0.148856124775343,1.,-2.02083464969897));
#32222=CARTESIAN_POINT('Ctrl Pts',(0.146965557332586,1.,-2.02666926182017));
#32223=CARTESIAN_POINT('Ctrl Pts',(0.145025140186058,1.,-2.03250223739941));
#32224=CARTESIAN_POINT('Ctrl Pts',(0.143035515058208,1.,-2.03832911025913));
#32225=CARTESIAN_POINT('Ctrl Pts',(0.140997332152545,1.,-2.04414757947919));
#32226=CARTESIAN_POINT('Ctrl Pts',(0.138911255368966,1.,-2.04995762001333));
#32227=CARTESIAN_POINT('Ctrl Pts',(0.136777941218044,1.,-2.0557604441427));
#32228=CARTESIAN_POINT('Ctrl Pts',(0.134598026192107,1.,-2.06155781517844));
#32229=CARTESIAN_POINT('Ctrl Pts',(0.13237211154771,1.,-2.06735123910319));
#32230=CARTESIAN_POINT('Ctrl Pts',(0.1301007483284,1.,-2.07314114713047));
#32231=CARTESIAN_POINT('Ctrl Pts',(0.127784445276116,1.,-2.07892715110967));
#32232=CARTESIAN_POINT('Ctrl Pts',(0.125423679412058,1.,-2.08470840653628));
#32233=CARTESIAN_POINT('Ctrl Pts',(0.123018905621083,1.,-2.09048392424826));
#32234=CARTESIAN_POINT('Ctrl Pts',(0.120570567965129,1.,-2.09625292867756));
#32235=CARTESIAN_POINT('Ctrl Pts',(0.118079107988368,1.,-2.10201512132945));
#32236=CARTESIAN_POINT('Ctrl Pts',(0.11554495768794,1.,-2.10777050261359));
#32237=CARTESIAN_POINT('Ctrl Pts',(0.112968534419746,1.,-2.11351924490335));
#32238=CARTESIAN_POINT('Ctrl Pts',(0.11035023613502,1.,-2.11926155590849));
#32239=CARTESIAN_POINT('Ctrl Pts',(0.107690435231068,1.,-2.12499752306927));
#32240=CARTESIAN_POINT('Ctrl Pts',(0.104989479152703,1.,-2.1307270488718));
#32241=CARTESIAN_POINT('Ctrl Pts',(0.102247700556064,1.,-2.13644992667052));
#32242=CARTESIAN_POINT('Ctrl Pts',(0.0994654261990743,1.,-2.14216588395974));
#32243=CARTESIAN_POINT('Ctrl Pts',(0.0966429852305689,1.,-2.14787463531864));
#32244=CARTESIAN_POINT('Ctrl Pts',(0.0937807218868345,1.,-2.15357593978377));
#32245=CARTESIAN_POINT('Ctrl Pts',(0.0908789888108266,1.,-2.15926961544808));
#32246=CARTESIAN_POINT('Ctrl Pts',(0.0879381291387823,1.,-2.16495552645275));
#32247=CARTESIAN_POINT('Ctrl Pts',(0.0849584620835643,1.,-2.17063357871031));
#32248=CARTESIAN_POINT('Ctrl Pts',(0.0819402680871939,1.,-2.1763037121106));
#32249=CARTESIAN_POINT('Ctrl Pts',(0.0788837727683228,1.,-2.18196589448304));
#32250=CARTESIAN_POINT('Ctrl Pts',(0.0757891465833411,1.,-2.1876201139874));
#32251=CARTESIAN_POINT('Ctrl Pts',(0.0732830357304276,1.,-2.19213712012956));
#32252=CARTESIAN_POINT('Ctrl Pts',(0.0713863779524627,1.,-2.19552129483562));
#32253=CARTESIAN_POINT('Ctrl Pts',(0.0701143536324926,1.,-2.19777582085261));
#32254=CARTESIAN_POINT('Ctrl Pts',(0.0694764450219584,1.,-2.19890268624765));
#32255=CARTESIAN_POINT('',(0.163289472382896,0.,-1.74236521665491));
#32256=CARTESIAN_POINT('Origin',(0.,0.,0.));
#32257=CARTESIAN_POINT('',(0.383122945602004,1.,-1.7075470150345));
#32258=CARTESIAN_POINT('Origin',(0.,1.,0.));
#32259=CARTESIAN_POINT('',(0.383122945602004,0.,-1.7075470150345));
#32260=CARTESIAN_POINT('Ctrl Pts',(0.61342227326009,-1.,-2.11275013067528));
#32261=CARTESIAN_POINT('Ctrl Pts',(0.61342227326009,1.,-2.11275013067528));
#32262=CARTESIAN_POINT('Ctrl Pts',(0.61246736556225,-1.,-2.11187554260142));
#32263=CARTESIAN_POINT('Ctrl Pts',(0.61246736556225,1.,-2.11187554260142));
#32264=CARTESIAN_POINT('Ctrl Pts',(0.610560911691113,-1.,-2.11012443807661));
#32265=CARTESIAN_POINT('Ctrl Pts',(0.610560911691113,1.,-2.11012443807661));
#32266=CARTESIAN_POINT('Ctrl Pts',(0.607711315456826,-1.,-2.10749199615859));
#32267=CARTESIAN_POINT('Ctrl Pts',(0.607711315456826,1.,-2.10749199615859));
#32268=CARTESIAN_POINT('Ctrl Pts',(0.603932030738212,-1.,-2.10397049887709));
#32269=CARTESIAN_POINT('Ctrl Pts',(0.603932030738212,1.,-2.10397049887709));
#32270=CARTESIAN_POINT('Ctrl Pts',(0.599241616422144,-1.,-2.09954930865331));
#32271=CARTESIAN_POINT('Ctrl Pts',(0.599241616422144,1.,-2.09954930865331));
#32272=CARTESIAN_POINT('Ctrl Pts',(0.594585006052823,-1.,-2.09510876220501));
#32273=CARTESIAN_POINT('Ctrl Pts',(0.594585006052823,1.,-2.09510876220501));
#32274=CARTESIAN_POINT('Ctrl Pts',(0.589962365403189,-1.,-2.09064881812053));
#32275=CARTESIAN_POINT('Ctrl Pts',(0.589962365403189,1.,-2.09064881812053));
#32276=CARTESIAN_POINT('Ctrl Pts',(0.585373918990895,-1.,-2.086169437277));
#32277=CARTESIAN_POINT('Ctrl Pts',(0.585373918990895,1.,-2.086169437277));
#32278=CARTESIAN_POINT('Ctrl Pts',(0.580819952107256,-1.,-2.08167059018138));
#32279=CARTESIAN_POINT('Ctrl Pts',(0.580819952107256,1.,-2.08167059018138));
#32280=CARTESIAN_POINT('Ctrl Pts',(0.576300797416274,-1.,-2.07715226767361));
#32281=CARTESIAN_POINT('Ctrl Pts',(0.576300797416274,1.,-2.07715226767361));
#32282=CARTESIAN_POINT('Ctrl Pts',(0.571816823242411,-1.,-2.07261449292758));
#32283=CARTESIAN_POINT('Ctrl Pts',(0.571816823242411,1.,-2.07261449292758));
#32284=CARTESIAN_POINT('Ctrl Pts',(0.567368421181229,-1.,-2.06805732997383));
#32285=CARTESIAN_POINT('Ctrl Pts',(0.567368421181229,1.,-2.06805732997383));
#32286=CARTESIAN_POINT('Ctrl Pts',(0.562955993082574,-1.,-2.06348090160697));
#32287=CARTESIAN_POINT('Ctrl Pts',(0.562955993082574,1.,-2.06348090160697));
#32288=CARTESIAN_POINT('Ctrl Pts',(0.558579940185467,-1.,-2.05888537756571));
#32289=CARTESIAN_POINT('Ctrl Pts',(0.558579940185467,1.,-2.05888537756571));
#32290=CARTESIAN_POINT('Ctrl Pts',(0.554240657464109,-1.,-2.05427091604482));
#32291=CARTESIAN_POINT('Ctrl Pts',(0.554240657464109,1.,-2.05427091604482));
#32292=CARTESIAN_POINT('Ctrl Pts',(0.549938525150342,-1.,-2.04963761077974));
#32293=CARTESIAN_POINT('Ctrl Pts',(0.549938525150342,1.,-2.04963761077974));
#32294=CARTESIAN_POINT('Ctrl Pts',(0.545673903817348,-1.,-2.0449854471456));
#32295=CARTESIAN_POINT('Ctrl Pts',(0.545673903817348,1.,-2.0449854471456));
#32296=CARTESIAN_POINT('Ctrl Pts',(0.54144712061552,-1.,-2.0403142269048));
#32297=CARTESIAN_POINT('Ctrl Pts',(0.54144712061552,1.,-2.0403142269048));
#32298=CARTESIAN_POINT('Ctrl Pts',(0.537258489833134,-1.,-2.03562362953993));
#32299=CARTESIAN_POINT('Ctrl Pts',(0.537258489833134,1.,-2.03562362953993));
#32300=CARTESIAN_POINT('Ctrl Pts',(0.533108355132905,-1.,-2.03091336214401));
#32301=CARTESIAN_POINT('Ctrl Pts',(0.533108355132905,1.,-2.03091336214401));
#32302=CARTESIAN_POINT('Ctrl Pts',(0.52899712724191,-1.,-2.02618329083289));
#32303=CARTESIAN_POINT('Ctrl Pts',(0.52899712724191,1.,-2.02618329083289));
#32304=CARTESIAN_POINT('Ctrl Pts',(0.524925318333518,-1.,-2.02143356304712));
#32305=CARTESIAN_POINT('Ctrl Pts',(0.524925318333518,1.,-2.02143356304712));
#32306=CARTESIAN_POINT('Ctrl Pts',(0.520893590399428,-1.,-2.01666477917306));
#32307=CARTESIAN_POINT('Ctrl Pts',(0.520893590399428,1.,-2.01666477917306));
#32308=CARTESIAN_POINT('Ctrl Pts',(0.516902681728733,-1.,-2.01187773939257));
#32309=CARTESIAN_POINT('Ctrl Pts',(0.516902681728733,1.,-2.01187773939257));
#32310=CARTESIAN_POINT('Ctrl Pts',(0.512953306961813,-1.,-2.00707309946955));
#32311=CARTESIAN_POINT('Ctrl Pts',(0.512953306961813,1.,-2.00707309946955));
#32312=CARTESIAN_POINT('Ctrl Pts',(0.509046069886152,-1.,-2.00225107134733));
#32313=CARTESIAN_POINT('Ctrl Pts',(0.509046069886152,1.,-2.00225107134733));
#32314=CARTESIAN_POINT('Ctrl Pts',(0.505181361323011,-1.,-1.99741107463567));
#32315=CARTESIAN_POINT('Ctrl Pts',(0.505181361323011,1.,-1.99741107463567));
#32316=CARTESIAN_POINT('Ctrl Pts',(0.501359287727129,-1.,-1.9925514912615));
#32317=CARTESIAN_POINT('Ctrl Pts',(0.501359287727129,1.,-1.9925514912615));
#32318=CARTESIAN_POINT('Ctrl Pts',(0.497579909545564,-1.,-1.98767044752929));
#32319=CARTESIAN_POINT('Ctrl Pts',(0.497579909545564,1.,-1.98767044752929));
#32320=CARTESIAN_POINT('Ctrl Pts',(0.493843476541492,-1.,-1.9827665876182));
#32321=CARTESIAN_POINT('Ctrl Pts',(0.493843476541492,1.,-1.9827665876182));
#32322=CARTESIAN_POINT('Ctrl Pts',(0.490150627860955,-1.,-1.97783973019229));
#32323=CARTESIAN_POINT('Ctrl Pts',(0.490150627860955,1.,-1.97783973019229));
#32324=CARTESIAN_POINT('Ctrl Pts',(0.486502692907661,-1.,-1.97289186263272));
#32325=CARTESIAN_POINT('Ctrl Pts',(0.486502692907661,1.,-1.97289186263272));
#32326=CARTESIAN_POINT('Ctrl Pts',(0.482901662120686,-1.,-1.96792703422358));
#32327=CARTESIAN_POINT('Ctrl Pts',(0.482901662120686,1.,-1.96792703422358));
#32328=CARTESIAN_POINT('Ctrl Pts',(0.479349583074846,-1.,-1.96294933055938));
#32329=CARTESIAN_POINT('Ctrl Pts',(0.479349583074846,1.,-1.96294933055938));
#32330=CARTESIAN_POINT('Ctrl Pts',(0.475848034683171,-1.,-1.95796111148175));
#32331=CARTESIAN_POINT('Ctrl Pts',(0.475848034683171,1.,-1.95796111148175));
#32332=CARTESIAN_POINT('Ctrl Pts',(0.472397672264079,-1.,-1.95296148278136));
#32333=CARTESIAN_POINT('Ctrl Pts',(0.472397672264079,1.,-1.95296148278136));
#32334=CARTESIAN_POINT('Ctrl Pts',(0.468997482913158,-1.,-1.94794381136524));
#32335=CARTESIAN_POINT('Ctrl Pts',(0.468997482913158,1.,-1.94794381136524));
#32336=CARTESIAN_POINT('Ctrl Pts',(0.465645462026064,-1.,-1.94289794196205));
#32337=CARTESIAN_POINT('Ctrl Pts',(0.465645462026064,1.,-1.94289794196205));
#32338=CARTESIAN_POINT('Ctrl Pts',(0.462340031009087,-1.,-1.93781486640834));
#32339=CARTESIAN_POINT('Ctrl Pts',(0.462340031009087,1.,-1.93781486640834));
#32340=CARTESIAN_POINT('Ctrl Pts',(0.459081234547931,-1.,-1.93269066517936));
#32341=CARTESIAN_POINT('Ctrl Pts',(0.459081234547931,1.,-1.93269066517936));
#32342=CARTESIAN_POINT('Ctrl Pts',(0.455872005174335,-1.,-1.92753067150461));
#32343=CARTESIAN_POINT('Ctrl Pts',(0.455872005174335,1.,-1.92753067150461));
#32344=CARTESIAN_POINT('Ctrl Pts',(0.452719478359356,-1.,-1.9223538064847));
#32345=CARTESIAN_POINT('Ctrl Pts',(0.452719478359356,1.,-1.9223538064847));
#32346=CARTESIAN_POINT('Ctrl Pts',(0.449632260106572,-1.,-1.91718342555717));
#32347=CARTESIAN_POINT('Ctrl Pts',(0.449632260106572,1.,-1.91718342555717));
#32348=CARTESIAN_POINT('Ctrl Pts',(0.446617343485651,-1.,-1.91203699981095));
#32349=CARTESIAN_POINT('Ctrl Pts',(0.446617343485651,1.,-1.91203699981095));
#32350=CARTESIAN_POINT('Ctrl Pts',(0.44367755684917,-1.,-1.90691756144906));
#32351=CARTESIAN_POINT('Ctrl Pts',(0.44367755684917,1.,-1.90691756144906));
#32352=CARTESIAN_POINT('Ctrl Pts',(0.44080783370416,-1.,-1.90180124389137));
#32353=CARTESIAN_POINT('Ctrl Pts',(0.44080783370416,1.,-1.90180124389137));
#32354=CARTESIAN_POINT('Ctrl Pts',(0.437995003948443,-1.,-1.89663648956549));
#32355=CARTESIAN_POINT('Ctrl Pts',(0.437995003948443,1.,-1.89663648956549));
#32356=CARTESIAN_POINT('Ctrl Pts',(0.43522566096358,-1.,-1.89136993975585));
#32357=CARTESIAN_POINT('Ctrl Pts',(0.43522566096358,1.,-1.89136993975585));
#32358=CARTESIAN_POINT('Ctrl Pts',(0.432493038548833,-1.,-1.88596913666828));
#32359=CARTESIAN_POINT('Ctrl Pts',(0.432493038548833,1.,-1.88596913666828));
#32360=CARTESIAN_POINT('Ctrl Pts',(0.429803062482217,-1.,-1.88044229001779));
#32361=CARTESIAN_POINT('Ctrl Pts',(0.429803062482217,1.,-1.88044229001779));
#32362=CARTESIAN_POINT('Ctrl Pts',(0.427183828518743,-1.,-1.87486989291334));
#32363=CARTESIAN_POINT('Ctrl Pts',(0.427183828518743,1.,-1.87486989291334));
#32364=CARTESIAN_POINT('Ctrl Pts',(0.424678177290876,-1.,-1.8693780394412));
#32365=CARTESIAN_POINT('Ctrl Pts',(0.424678177290876,1.,-1.8693780394412));
#32366=CARTESIAN_POINT('Ctrl Pts',(0.422327307417884,-1.,-1.86408083333863));
#32367=CARTESIAN_POINT('Ctrl Pts',(0.422327307417884,1.,-1.86408083333863));
#32368=CARTESIAN_POINT('Ctrl Pts',(0.420157287975583,-1.,-1.8590328109667));
#32369=CARTESIAN_POINT('Ctrl Pts',(0.420157287975583,1.,-1.8590328109667));
#32370=CARTESIAN_POINT('Ctrl Pts',(0.418164129144045,-1.,-1.8541763285645));
#32371=CARTESIAN_POINT('Ctrl Pts',(0.418164129144045,1.,-1.8541763285645));
#32372=CARTESIAN_POINT('Ctrl Pts',(0.416300022039885,-1.,-1.84929312930314));
#32373=CARTESIAN_POINT('Ctrl Pts',(0.416300022039885,1.,-1.84929312930314));
#32374=CARTESIAN_POINT('Ctrl Pts',(0.414487438255542,-1.,-1.84405757074218));
#32375=CARTESIAN_POINT('Ctrl Pts',(0.414487438255542,1.,-1.84405757074218));
#32376=CARTESIAN_POINT('Ctrl Pts',(0.412633125322945,-1.,-1.8380895347617));
#32377=CARTESIAN_POINT('Ctrl Pts',(0.412633125322945,1.,-1.8380895347617));
#32378=CARTESIAN_POINT('Ctrl Pts',(0.410641256301276,-1.,-1.83100408895047));
#32379=CARTESIAN_POINT('Ctrl Pts',(0.410641256301276,1.,-1.83100408895047));
#32380=CARTESIAN_POINT('Ctrl Pts',(0.408428948106227,-1.,-1.82247022677562));
#32381=CARTESIAN_POINT('Ctrl Pts',(0.408428948106227,1.,-1.82247022677562));
#32382=CARTESIAN_POINT('Ctrl Pts',(0.405933518407175,-1.,-1.81223801812013));
#32383=CARTESIAN_POINT('Ctrl Pts',(0.405933518407175,1.,-1.81223801812013));
#32384=CARTESIAN_POINT('Ctrl Pts',(0.403107976163396,-1.,-1.80012077173238));
#32385=CARTESIAN_POINT('Ctrl Pts',(0.403107976163396,1.,-1.80012077173238));
#32386=CARTESIAN_POINT('Ctrl Pts',(0.399919403774155,-1.,-1.78598826343754));
#32387=CARTESIAN_POINT('Ctrl Pts',(0.399919403774155,1.,-1.78598826343754));
#32388=CARTESIAN_POINT('Ctrl Pts',(0.396346196110688,-1.,-1.76975560043442));
#32389=CARTESIAN_POINT('Ctrl Pts',(0.396346196110688,1.,-1.76975560043442));
#32390=CARTESIAN_POINT('Ctrl Pts',(0.392375812285395,-1.,-1.75137405310193));
#32391=CARTESIAN_POINT('Ctrl Pts',(0.392375812285395,1.,-1.75137405310193));
#32392=CARTESIAN_POINT('Ctrl Pts',(0.388877023502615,-1.,-1.73493170972829));
#32393=CARTESIAN_POINT('Ctrl Pts',(0.388877023502615,1.,-1.73493170972829));
#32394=CARTESIAN_POINT('Ctrl Pts',(0.386070790323281,-1.,-1.72162022244582));
#32395=CARTESIAN_POINT('Ctrl Pts',(0.386070790323281,1.,-1.72162022244582));
#32396=CARTESIAN_POINT('Ctrl Pts',(0.384119047314215,-1.,-1.71231062891398));
#32397=CARTESIAN_POINT('Ctrl Pts',(0.384119047314215,1.,-1.71231062891398));
#32398=CARTESIAN_POINT('Ctrl Pts',(0.383122945602004,-1.,-1.7075470150345));
#32399=CARTESIAN_POINT('Ctrl Pts',(0.383122945602004,1.,-1.7075470150345));
#32400=CARTESIAN_POINT('',(0.61342227326009,1.,-2.11275013067528));
#32401=CARTESIAN_POINT('Ctrl Pts',(0.61342227326009,1.,-2.11275013067528));
#32402=CARTESIAN_POINT('Ctrl Pts',(0.61246736556225,1.,-2.11187554260142));
#32403=CARTESIAN_POINT('Ctrl Pts',(0.610560911691113,1.,-2.11012443807661));
#32404=CARTESIAN_POINT('Ctrl Pts',(0.607711315456826,1.,-2.10749199615859));
#32405=CARTESIAN_POINT('Ctrl Pts',(0.603932030738212,1.,-2.10397049887709));
#32406=CARTESIAN_POINT('Ctrl Pts',(0.599241616422144,1.,-2.09954930865331));
#32407=CARTESIAN_POINT('Ctrl Pts',(0.594585006052823,1.,-2.09510876220501));
#32408=CARTESIAN_POINT('Ctrl Pts',(0.589962365403189,1.,-2.09064881812053));
#32409=CARTESIAN_POINT('Ctrl Pts',(0.585373918990895,1.,-2.086169437277));
#32410=CARTESIAN_POINT('Ctrl Pts',(0.580819952107256,1.,-2.08167059018138));
#32411=CARTESIAN_POINT('Ctrl Pts',(0.576300797416274,1.,-2.07715226767361));
#32412=CARTESIAN_POINT('Ctrl Pts',(0.571816823242411,1.,-2.07261449292758));
#32413=CARTESIAN_POINT('Ctrl Pts',(0.567368421181229,1.,-2.06805732997383));
#32414=CARTESIAN_POINT('Ctrl Pts',(0.562955993082574,1.,-2.06348090160697));
#32415=CARTESIAN_POINT('Ctrl Pts',(0.558579940185467,1.,-2.05888537756571));
#32416=CARTESIAN_POINT('Ctrl Pts',(0.554240657464109,1.,-2.05427091604482));
#32417=CARTESIAN_POINT('Ctrl Pts',(0.549938525150342,1.,-2.04963761077974));
#32418=CARTESIAN_POINT('Ctrl Pts',(0.545673903817348,1.,-2.0449854471456));
#32419=CARTESIAN_POINT('Ctrl Pts',(0.54144712061552,1.,-2.0403142269048));
#32420=CARTESIAN_POINT('Ctrl Pts',(0.537258489833134,1.,-2.03562362953993));
#32421=CARTESIAN_POINT('Ctrl Pts',(0.533108355132905,1.,-2.03091336214401));
#32422=CARTESIAN_POINT('Ctrl Pts',(0.52899712724191,1.,-2.02618329083289));
#32423=CARTESIAN_POINT('Ctrl Pts',(0.524925318333518,1.,-2.02143356304712));
#32424=CARTESIAN_POINT('Ctrl Pts',(0.520893590399428,1.,-2.01666477917306));
#32425=CARTESIAN_POINT('Ctrl Pts',(0.516902681728733,1.,-2.01187773939257));
#32426=CARTESIAN_POINT('Ctrl Pts',(0.512953306961813,1.,-2.00707309946955));
#32427=CARTESIAN_POINT('Ctrl Pts',(0.509046069886152,1.,-2.00225107134733));
#32428=CARTESIAN_POINT('Ctrl Pts',(0.505181361323011,1.,-1.99741107463567));
#32429=CARTESIAN_POINT('Ctrl Pts',(0.501359287727129,1.,-1.9925514912615));
#32430=CARTESIAN_POINT('Ctrl Pts',(0.497579909545564,1.,-1.98767044752929));
#32431=CARTESIAN_POINT('Ctrl Pts',(0.493843476541492,1.,-1.9827665876182));
#32432=CARTESIAN_POINT('Ctrl Pts',(0.490150627860955,1.,-1.97783973019229));
#32433=CARTESIAN_POINT('Ctrl Pts',(0.486502692907661,1.,-1.97289186263272));
#32434=CARTESIAN_POINT('Ctrl Pts',(0.482901662120686,1.,-1.96792703422358));
#32435=CARTESIAN_POINT('Ctrl Pts',(0.479349583074846,1.,-1.96294933055938));
#32436=CARTESIAN_POINT('Ctrl Pts',(0.475848034683171,1.,-1.95796111148175));
#32437=CARTESIAN_POINT('Ctrl Pts',(0.472397672264079,1.,-1.95296148278136));
#32438=CARTESIAN_POINT('Ctrl Pts',(0.468997482913158,1.,-1.94794381136524));
#32439=CARTESIAN_POINT('Ctrl Pts',(0.465645462026064,1.,-1.94289794196205));
#32440=CARTESIAN_POINT('Ctrl Pts',(0.462340031009087,1.,-1.93781486640834));
#32441=CARTESIAN_POINT('Ctrl Pts',(0.459081234547931,1.,-1.93269066517936));
#32442=CARTESIAN_POINT('Ctrl Pts',(0.455872005174335,1.,-1.92753067150461));
#32443=CARTESIAN_POINT('Ctrl Pts',(0.452719478359356,1.,-1.9223538064847));
#32444=CARTESIAN_POINT('Ctrl Pts',(0.449632260106572,1.,-1.91718342555717));
#32445=CARTESIAN_POINT('Ctrl Pts',(0.446617343485651,1.,-1.91203699981095));
#32446=CARTESIAN_POINT('Ctrl Pts',(0.44367755684917,1.,-1.90691756144906));
#32447=CARTESIAN_POINT('Ctrl Pts',(0.44080783370416,1.,-1.90180124389137));
#32448=CARTESIAN_POINT('Ctrl Pts',(0.437995003948443,1.,-1.89663648956549));
#32449=CARTESIAN_POINT('Ctrl Pts',(0.43522566096358,1.,-1.89136993975585));
#32450=CARTESIAN_POINT('Ctrl Pts',(0.432493038548833,1.,-1.88596913666828));
#32451=CARTESIAN_POINT('Ctrl Pts',(0.429803062482217,1.,-1.88044229001779));
#32452=CARTESIAN_POINT('Ctrl Pts',(0.427183828518743,1.,-1.87486989291334));
#32453=CARTESIAN_POINT('Ctrl Pts',(0.424678177290876,1.,-1.8693780394412));
#32454=CARTESIAN_POINT('Ctrl Pts',(0.422327307417884,1.,-1.86408083333863));
#32455=CARTESIAN_POINT('Ctrl Pts',(0.420157287975583,1.,-1.8590328109667));
#32456=CARTESIAN_POINT('Ctrl Pts',(0.418164129144045,1.,-1.8541763285645));
#32457=CARTESIAN_POINT('Ctrl Pts',(0.416300022039885,1.,-1.84929312930314));
#32458=CARTESIAN_POINT('Ctrl Pts',(0.414487438255542,1.,-1.84405757074218));
#32459=CARTESIAN_POINT('Ctrl Pts',(0.412633125322945,1.,-1.8380895347617));
#32460=CARTESIAN_POINT('Ctrl Pts',(0.410641256301276,1.,-1.83100408895047));
#32461=CARTESIAN_POINT('Ctrl Pts',(0.408428948106227,1.,-1.82247022677562));
#32462=CARTESIAN_POINT('Ctrl Pts',(0.405933518407175,1.,-1.81223801812013));
#32463=CARTESIAN_POINT('Ctrl Pts',(0.403107976163396,1.,-1.80012077173238));
#32464=CARTESIAN_POINT('Ctrl Pts',(0.399919403774155,1.,-1.78598826343754));
#32465=CARTESIAN_POINT('Ctrl Pts',(0.396346196110688,1.,-1.76975560043442));
#32466=CARTESIAN_POINT('Ctrl Pts',(0.392375812285395,1.,-1.75137405310193));
#32467=CARTESIAN_POINT('Ctrl Pts',(0.388877023502615,1.,-1.73493170972829));
#32468=CARTESIAN_POINT('Ctrl Pts',(0.386070790323281,1.,-1.72162022244582));
#32469=CARTESIAN_POINT('Ctrl Pts',(0.384119047314215,1.,-1.71231062891398));
#32470=CARTESIAN_POINT('Ctrl Pts',(0.383122945602004,1.,-1.7075470150345));
#32471=CARTESIAN_POINT('',(0.61342227326009,0.,-2.11275013067528));
#32472=CARTESIAN_POINT('Origin',(0.745574324794401,0.,-2.0698113262342));
#32473=CARTESIAN_POINT('',(0.745574324794401,1.,-2.0698113262342));
#32474=CARTESIAN_POINT('',(0.61342227326009,1.,-2.11275013067528));
#32475=CARTESIAN_POINT('',(0.745574324794401,0.,-2.0698113262342));
#32476=CARTESIAN_POINT('Ctrl Pts',(0.693717979106306,-1.,-1.60662857109684));
#32477=CARTESIAN_POINT('Ctrl Pts',(0.693717979106306,1.,-1.60662857109684));
#32478=CARTESIAN_POINT('Ctrl Pts',(0.695712097881194,-1.,-1.61106790958151));
#32479=CARTESIAN_POINT('Ctrl Pts',(0.695712097881194,1.,-1.61106790958151));
#32480=CARTESIAN_POINT('Ctrl Pts',(0.699605146405088,-1.,-1.61974673472612));
#32481=CARTESIAN_POINT('Ctrl Pts',(0.699605146405088,1.,-1.61974673472612));
#32482=CARTESIAN_POINT('Ctrl Pts',(0.705159151988319,-1.,-1.63216541664676));
#32483=CARTESIAN_POINT('Ctrl Pts',(0.705159151988319,1.,-1.63216541664676));
#32484=CARTESIAN_POINT('Ctrl Pts',(0.711993139355394,-1.,-1.64752408832016));
#32485=CARTESIAN_POINT('Ctrl Pts',(0.711993139355394,1.,-1.64752408832016));
#32486=CARTESIAN_POINT('Ctrl Pts',(0.719585433804282,-1.,-1.6647288055568));
#32487=CARTESIAN_POINT('Ctrl Pts',(0.719585433804282,1.,-1.6647288055568));
#32488=CARTESIAN_POINT('Ctrl Pts',(0.726235967997433,-1.,-1.67996158455503));
#32489=CARTESIAN_POINT('Ctrl Pts',(0.726235967997433,1.,-1.67996158455503));
#32490=CARTESIAN_POINT('Ctrl Pts',(0.731963238697195,-1.,-1.69326921975743));
#32491=CARTESIAN_POINT('Ctrl Pts',(0.731963238697195,1.,-1.69326921975743));
#32492=CARTESIAN_POINT('Ctrl Pts',(0.736799665724771,-1.,-1.70473309006121));
#32493=CARTESIAN_POINT('Ctrl Pts',(0.736799665724771,1.,-1.70473309006121));
#32494=CARTESIAN_POINT('Ctrl Pts',(0.740795162032087,-1.,-1.71447789751927));
#32495=CARTESIAN_POINT('Ctrl Pts',(0.740795162032087,1.,-1.71447789751927));
#32496=CARTESIAN_POINT('Ctrl Pts',(0.744021445433764,-1.,-1.7226822991693));
#32497=CARTESIAN_POINT('Ctrl Pts',(0.744021445433764,1.,-1.7226822991693));
#32498=CARTESIAN_POINT('Ctrl Pts',(0.746574710096436,-1.,-1.72958533647399));
#32499=CARTESIAN_POINT('Ctrl Pts',(0.746574710096436,1.,-1.72958533647399));
#32500=CARTESIAN_POINT('Ctrl Pts',(0.748582462954854,-1.,-1.73550351679848));
#32501=CARTESIAN_POINT('Ctrl Pts',(0.748582462954854,1.,-1.73550351679848));
#32502=CARTESIAN_POINT('Ctrl Pts',(0.75019343597954,-1.,-1.74080458266705));
#32503=CARTESIAN_POINT('Ctrl Pts',(0.75019343597954,1.,-1.74080458266705));
#32504=CARTESIAN_POINT('Ctrl Pts',(0.751555614163629,-1.,-1.74585086852298));
#32505=CARTESIAN_POINT('Ctrl Pts',(0.751555614163629,1.,-1.74585086852298));
#32506=CARTESIAN_POINT('Ctrl Pts',(0.752797683531377,-1.,-1.75095139468809));
#32507=CARTESIAN_POINT('Ctrl Pts',(0.752797683531377,1.,-1.75095139468809));
#32508=CARTESIAN_POINT('Ctrl Pts',(0.75400925402848,-1.,-1.75631083600175));
#32509=CARTESIAN_POINT('Ctrl Pts',(0.75400925402848,1.,-1.75631083600175));
#32510=CARTESIAN_POINT('Ctrl Pts',(0.755220979975262,-1.,-1.7619781724032));
#32511=CARTESIAN_POINT('Ctrl Pts',(0.755220979975262,1.,-1.7619781724032));
#32512=CARTESIAN_POINT('Ctrl Pts',(0.756421896028403,-1.,-1.76789396003141));
#32513=CARTESIAN_POINT('Ctrl Pts',(0.756421896028403,1.,-1.76789396003141));
#32514=CARTESIAN_POINT('Ctrl Pts',(0.757578264077238,-1.,-1.77394167108342));
#32515=CARTESIAN_POINT('Ctrl Pts',(0.757578264077238,1.,-1.77394167108342));
#32516=CARTESIAN_POINT('Ctrl Pts',(0.75865062667738,-1.,-1.77999411220912));
#32517=CARTESIAN_POINT('Ctrl Pts',(0.75865062667738,1.,-1.77999411220912));
#32518=CARTESIAN_POINT('Ctrl Pts',(0.759614401109868,-1.,-1.78596964884527));
#32519=CARTESIAN_POINT('Ctrl Pts',(0.759614401109868,1.,-1.78596964884527));
#32520=CARTESIAN_POINT('Ctrl Pts',(0.760469555880425,-1.,-1.79185815610802));
#32521=CARTESIAN_POINT('Ctrl Pts',(0.760469555880425,1.,-1.79185815610802));
#32522=CARTESIAN_POINT('Ctrl Pts',(0.761229695230359,-1.,-1.79768986997735));
#32523=CARTESIAN_POINT('Ctrl Pts',(0.761229695230359,1.,-1.79768986997735));
#32524=CARTESIAN_POINT('Ctrl Pts',(0.761915336443515,-1.,-1.80351583877334));
#32525=CARTESIAN_POINT('Ctrl Pts',(0.761915336443515,1.,-1.80351583877334));
#32526=CARTESIAN_POINT('Ctrl Pts',(0.762546129464036,-1.,-1.80938551463989));
#32527=CARTESIAN_POINT('Ctrl Pts',(0.762546129464036,1.,-1.80938551463989));
#32528=CARTESIAN_POINT('Ctrl Pts',(0.763132003836783,-1.,-1.81532118405566));
#32529=CARTESIAN_POINT('Ctrl Pts',(0.763132003836783,1.,-1.81532118405566));
#32530=CARTESIAN_POINT('Ctrl Pts',(0.763673465462854,-1.,-1.82131873145297));
#32531=CARTESIAN_POINT('Ctrl Pts',(0.763673465462854,1.,-1.82131873145297));
#32532=CARTESIAN_POINT('Ctrl Pts',(0.764165902606055,-1.,-1.8273599120008));
#32533=CARTESIAN_POINT('Ctrl Pts',(0.764165902606055,1.,-1.8273599120008));
#32534=CARTESIAN_POINT('Ctrl Pts',(0.764602549687845,-1.,-1.8334207722714));
#32535=CARTESIAN_POINT('Ctrl Pts',(0.764602549687845,1.,-1.8334207722714));
#32536=CARTESIAN_POINT('Ctrl Pts',(0.764978057881687,-1.,-1.83948181064823));
#32537=CARTESIAN_POINT('Ctrl Pts',(0.764978057881687,1.,-1.83948181064823));
#32538=CARTESIAN_POINT('Ctrl Pts',(0.765291664861971,-1.,-1.84553698875911));
#32539=CARTESIAN_POINT('Ctrl Pts',(0.765291664861971,1.,-1.84553698875911));
#32540=CARTESIAN_POINT('Ctrl Pts',(0.765545710619023,-1.,-1.85158945130054));
#32541=CARTESIAN_POINT('Ctrl Pts',(0.765545710619023,1.,-1.85158945130054));
#32542=CARTESIAN_POINT('Ctrl Pts',(0.765744212909305,-1.,-1.85764741390391));
#32543=CARTESIAN_POINT('Ctrl Pts',(0.765744212909305,1.,-1.85764741390391));
#32544=CARTESIAN_POINT('Ctrl Pts',(0.765891519092557,-1.,-1.86372027063315));
#32545=CARTESIAN_POINT('Ctrl Pts',(0.765891519092557,1.,-1.86372027063315));
#32546=CARTESIAN_POINT('Ctrl Pts',(0.765990708546111,-1.,-1.86981398314345));
#32547=CARTESIAN_POINT('Ctrl Pts',(0.765990708546111,1.,-1.86981398314345));
#32548=CARTESIAN_POINT('Ctrl Pts',(0.766042837036759,-1.,-1.87592888967886));
#32549=CARTESIAN_POINT('Ctrl Pts',(0.766042837036759,1.,-1.87592888967886));
#32550=CARTESIAN_POINT('Ctrl Pts',(0.766047794851868,-1.,-1.88206215302561));
#32551=CARTESIAN_POINT('Ctrl Pts',(0.766047794851868,1.,-1.88206215302561));
#32552=CARTESIAN_POINT('Ctrl Pts',(0.76600483706209,-1.,-1.88820926433409));
#32553=CARTESIAN_POINT('Ctrl Pts',(0.76600483706209,1.,-1.88820926433409));
#32554=CARTESIAN_POINT('Ctrl Pts',(0.765913193856979,-1.,-1.89436577771389));
#32555=CARTESIAN_POINT('Ctrl Pts',(0.765913193856979,1.,-1.89436577771389));
#32556=CARTESIAN_POINT('Ctrl Pts',(0.765772772593395,-1.,-1.90052930393599));
#32557=CARTESIAN_POINT('Ctrl Pts',(0.765772772593395,1.,-1.90052930393599));
#32558=CARTESIAN_POINT('Ctrl Pts',(0.765584196937936,-1.,-1.90669961402362));
#32559=CARTESIAN_POINT('Ctrl Pts',(0.765584196937936,1.,-1.90669961402362));
#32560=CARTESIAN_POINT('Ctrl Pts',(0.765348465884739,-1.,-1.91287765805174));
#32561=CARTESIAN_POINT('Ctrl Pts',(0.765348465884739,1.,-1.91287765805174));
#32562=CARTESIAN_POINT('Ctrl Pts',(0.765066729667095,-1.,-1.91906491634197));
#32563=CARTESIAN_POINT('Ctrl Pts',(0.765066729667095,1.,-1.91906491634197));
#32564=CARTESIAN_POINT('Ctrl Pts',(0.764740025488189,-1.,-1.92526263537041));
#32565=CARTESIAN_POINT('Ctrl Pts',(0.764740025488189,1.,-1.92526263537041));
#32566=CARTESIAN_POINT('Ctrl Pts',(0.764369010673889,-1.,-1.93147105496367));
#32567=CARTESIAN_POINT('Ctrl Pts',(0.764369010673889,1.,-1.93147105496367));
#32568=CARTESIAN_POINT('Ctrl Pts',(0.763954049121393,-1.,-1.93768964875867));
#32569=CARTESIAN_POINT('Ctrl Pts',(0.763954049121393,1.,-1.93768964875867));
#32570=CARTESIAN_POINT('Ctrl Pts',(0.76349533353858,-1.,-1.94391746617626));
#32571=CARTESIAN_POINT('Ctrl Pts',(0.76349533353858,1.,-1.94391746617626));
#32572=CARTESIAN_POINT('Ctrl Pts',(0.762992990878774,-1.,-1.95015342590025));
#32573=CARTESIAN_POINT('Ctrl Pts',(0.762992990878774,1.,-1.95015342590025));
#32574=CARTESIAN_POINT('Ctrl Pts',(0.762447203806263,-1.,-1.95639665309893));
#32575=CARTESIAN_POINT('Ctrl Pts',(0.762447203806263,1.,-1.95639665309893));
#32576=CARTESIAN_POINT('Ctrl Pts',(0.761858300014575,-1.,-1.96264672744229));
#32577=CARTESIAN_POINT('Ctrl Pts',(0.761858300014575,1.,-1.96264672744229));
#32578=CARTESIAN_POINT('Ctrl Pts',(0.761226690483986,-1.,-1.96890351582545));
#32579=CARTESIAN_POINT('Ctrl Pts',(0.761226690483986,1.,-1.96890351582545));
#32580=CARTESIAN_POINT('Ctrl Pts',(0.760552825409855,-1.,-1.97516705321521));
#32581=CARTESIAN_POINT('Ctrl Pts',(0.760552825409855,1.,-1.97516705321521));
#32582=CARTESIAN_POINT('Ctrl Pts',(0.759837147452135,-1.,-1.98143741418156));
#32583=CARTESIAN_POINT('Ctrl Pts',(0.759837147452135,1.,-1.98143741418156));
#32584=CARTESIAN_POINT('Ctrl Pts',(0.759080037802242,-1.,-1.98771456680806));
#32585=CARTESIAN_POINT('Ctrl Pts',(0.759080037802242,1.,-1.98771456680806));
#32586=CARTESIAN_POINT('Ctrl Pts',(0.758281796766377,-1.,-1.9939983109871));
#32587=CARTESIAN_POINT('Ctrl Pts',(0.758281796766377,1.,-1.9939983109871));
#32588=CARTESIAN_POINT('Ctrl Pts',(0.757442676862341,-1.,-2.00028834739072));
#32589=CARTESIAN_POINT('Ctrl Pts',(0.757442676862341,1.,-2.00028834739072));
#32590=CARTESIAN_POINT('Ctrl Pts',(0.756562904646496,-1.,-2.00658431587682));
#32591=CARTESIAN_POINT('Ctrl Pts',(0.756562904646496,1.,-2.00658431587682));
#32592=CARTESIAN_POINT('Ctrl Pts',(0.7556427049581,-1.,-2.01288584328149));
#32593=CARTESIAN_POINT('Ctrl Pts',(0.7556427049581,1.,-2.01288584328149));
#32594=CARTESIAN_POINT('Ctrl Pts',(0.75468233072352,-1.,-2.01919259406003));
#32595=CARTESIAN_POINT('Ctrl Pts',(0.75468233072352,1.,-2.01919259406003));
#32596=CARTESIAN_POINT('Ctrl Pts',(0.753682061113765,-1.,-2.02550428623587));
#32597=CARTESIAN_POINT('Ctrl Pts',(0.753682061113765,1.,-2.02550428623587));
#32598=CARTESIAN_POINT('Ctrl Pts',(0.752642180488104,-1.,-2.03182068456467));
#32599=CARTESIAN_POINT('Ctrl Pts',(0.752642180488104,1.,-2.03182068456467));
#32600=CARTESIAN_POINT('Ctrl Pts',(0.751562963361383,-1.,-2.03814160092173));
#32601=CARTESIAN_POINT('Ctrl Pts',(0.751562963361383,1.,-2.03814160092173));
#32602=CARTESIAN_POINT('Ctrl Pts',(0.750444657874758,-1.,-2.04446689147754));
#32603=CARTESIAN_POINT('Ctrl Pts',(0.750444657874758,1.,-2.04446689147754));
#32604=CARTESIAN_POINT('Ctrl Pts',(0.749287468663053,-1.,-2.05079645591606));
#32605=CARTESIAN_POINT('Ctrl Pts',(0.749287468663053,1.,-2.05079645591606));
#32606=CARTESIAN_POINT('Ctrl Pts',(0.748091554181101,-1.,-2.05713023030263));
#32607=CARTESIAN_POINT('Ctrl Pts',(0.748091554181101,1.,-2.05713023030263));
#32608=CARTESIAN_POINT('Ctrl Pts',(0.747103932785504,-1.,-2.06220058927162));
#32609=CARTESIAN_POINT('Ctrl Pts',(0.747103932785504,1.,-2.06220058927162));
#32610=CARTESIAN_POINT('Ctrl Pts',(0.746345871542695,-1.,-2.06600523016401));
#32611=CARTESIAN_POINT('Ctrl Pts',(0.746345871542695,1.,-2.06600523016401));
#32612=CARTESIAN_POINT('Ctrl Pts',(0.74583279137781,-1.,-2.06854248895575));
#32613=CARTESIAN_POINT('Ctrl Pts',(0.74583279137781,1.,-2.06854248895575));
#32614=CARTESIAN_POINT('Ctrl Pts',(0.745574324794401,-1.,-2.0698113262342));
#32615=CARTESIAN_POINT('Ctrl Pts',(0.745574324794401,1.,-2.0698113262342));
#32616=CARTESIAN_POINT('',(0.693717979106306,1.,-1.60662857109684));
#32617=CARTESIAN_POINT('Ctrl Pts',(0.693717979106306,1.,-1.60662857109684));
#32618=CARTESIAN_POINT('Ctrl Pts',(0.695712097881194,1.,-1.61106790958151));
#32619=CARTESIAN_POINT('Ctrl Pts',(0.699605146405088,1.,-1.61974673472612));
#32620=CARTESIAN_POINT('Ctrl Pts',(0.705159151988319,1.,-1.63216541664676));
#32621=CARTESIAN_POINT('Ctrl Pts',(0.711993139355394,1.,-1.64752408832016));
#32622=CARTESIAN_POINT('Ctrl Pts',(0.719585433804282,1.,-1.6647288055568));
#32623=CARTESIAN_POINT('Ctrl Pts',(0.726235967997433,1.,-1.67996158455503));
#32624=CARTESIAN_POINT('Ctrl Pts',(0.731963238697195,1.,-1.69326921975743));
#32625=CARTESIAN_POINT('Ctrl Pts',(0.736799665724771,1.,-1.70473309006121));
#32626=CARTESIAN_POINT('Ctrl Pts',(0.740795162032087,1.,-1.71447789751927));
#32627=CARTESIAN_POINT('Ctrl Pts',(0.744021445433764,1.,-1.7226822991693));
#32628=CARTESIAN_POINT('Ctrl Pts',(0.746574710096436,1.,-1.72958533647399));
#32629=CARTESIAN_POINT('Ctrl Pts',(0.748582462954854,1.,-1.73550351679848));
#32630=CARTESIAN_POINT('Ctrl Pts',(0.75019343597954,1.,-1.74080458266705));
#32631=CARTESIAN_POINT('Ctrl Pts',(0.751555614163629,1.,-1.74585086852298));
#32632=CARTESIAN_POINT('Ctrl Pts',(0.752797683531377,1.,-1.75095139468809));
#32633=CARTESIAN_POINT('Ctrl Pts',(0.75400925402848,1.,-1.75631083600175));
#32634=CARTESIAN_POINT('Ctrl Pts',(0.755220979975262,1.,-1.7619781724032));
#32635=CARTESIAN_POINT('Ctrl Pts',(0.756421896028403,1.,-1.76789396003141));
#32636=CARTESIAN_POINT('Ctrl Pts',(0.757578264077238,1.,-1.77394167108342));
#32637=CARTESIAN_POINT('Ctrl Pts',(0.75865062667738,1.,-1.77999411220912));
#32638=CARTESIAN_POINT('Ctrl Pts',(0.759614401109868,1.,-1.78596964884527));
#32639=CARTESIAN_POINT('Ctrl Pts',(0.760469555880425,1.,-1.79185815610802));
#32640=CARTESIAN_POINT('Ctrl Pts',(0.761229695230359,1.,-1.79768986997735));
#32641=CARTESIAN_POINT('Ctrl Pts',(0.761915336443515,1.,-1.80351583877334));
#32642=CARTESIAN_POINT('Ctrl Pts',(0.762546129464036,1.,-1.80938551463989));
#32643=CARTESIAN_POINT('Ctrl Pts',(0.763132003836783,1.,-1.81532118405566));
#32644=CARTESIAN_POINT('Ctrl Pts',(0.763673465462854,1.,-1.82131873145297));
#32645=CARTESIAN_POINT('Ctrl Pts',(0.764165902606055,1.,-1.8273599120008));
#32646=CARTESIAN_POINT('Ctrl Pts',(0.764602549687845,1.,-1.8334207722714));
#32647=CARTESIAN_POINT('Ctrl Pts',(0.764978057881687,1.,-1.83948181064823));
#32648=CARTESIAN_POINT('Ctrl Pts',(0.765291664861971,1.,-1.84553698875911));
#32649=CARTESIAN_POINT('Ctrl Pts',(0.765545710619023,1.,-1.85158945130054));
#32650=CARTESIAN_POINT('Ctrl Pts',(0.765744212909305,1.,-1.85764741390391));
#32651=CARTESIAN_POINT('Ctrl Pts',(0.765891519092557,1.,-1.86372027063315));
#32652=CARTESIAN_POINT('Ctrl Pts',(0.765990708546111,1.,-1.86981398314345));
#32653=CARTESIAN_POINT('Ctrl Pts',(0.766042837036759,1.,-1.87592888967886));
#32654=CARTESIAN_POINT('Ctrl Pts',(0.766047794851868,1.,-1.88206215302561));
#32655=CARTESIAN_POINT('Ctrl Pts',(0.76600483706209,1.,-1.88820926433409));
#32656=CARTESIAN_POINT('Ctrl Pts',(0.765913193856979,1.,-1.89436577771389));
#32657=CARTESIAN_POINT('Ctrl Pts',(0.765772772593395,1.,-1.90052930393599));
#32658=CARTESIAN_POINT('Ctrl Pts',(0.765584196937936,1.,-1.90669961402362));
#32659=CARTESIAN_POINT('Ctrl Pts',(0.765348465884739,1.,-1.91287765805174));
#32660=CARTESIAN_POINT('Ctrl Pts',(0.765066729667095,1.,-1.91906491634197));
#32661=CARTESIAN_POINT('Ctrl Pts',(0.764740025488189,1.,-1.92526263537041));
#32662=CARTESIAN_POINT('Ctrl Pts',(0.764369010673889,1.,-1.93147105496367));
#32663=CARTESIAN_POINT('Ctrl Pts',(0.763954049121393,1.,-1.93768964875867));
#32664=CARTESIAN_POINT('Ctrl Pts',(0.76349533353858,1.,-1.94391746617626));
#32665=CARTESIAN_POINT('Ctrl Pts',(0.762992990878774,1.,-1.95015342590025));
#32666=CARTESIAN_POINT('Ctrl Pts',(0.762447203806263,1.,-1.95639665309893));
#32667=CARTESIAN_POINT('Ctrl Pts',(0.761858300014575,1.,-1.96264672744229));
#32668=CARTESIAN_POINT('Ctrl Pts',(0.761226690483986,1.,-1.96890351582545));
#32669=CARTESIAN_POINT('Ctrl Pts',(0.760552825409855,1.,-1.97516705321521));
#32670=CARTESIAN_POINT('Ctrl Pts',(0.759837147452135,1.,-1.98143741418156));
#32671=CARTESIAN_POINT('Ctrl Pts',(0.759080037802242,1.,-1.98771456680806));
#32672=CARTESIAN_POINT('Ctrl Pts',(0.758281796766377,1.,-1.9939983109871));
#32673=CARTESIAN_POINT('Ctrl Pts',(0.757442676862341,1.,-2.00028834739072));
#32674=CARTESIAN_POINT('Ctrl Pts',(0.756562904646496,1.,-2.00658431587682));
#32675=CARTESIAN_POINT('Ctrl Pts',(0.7556427049581,1.,-2.01288584328149));
#32676=CARTESIAN_POINT('Ctrl Pts',(0.75468233072352,1.,-2.01919259406003));
#32677=CARTESIAN_POINT('Ctrl Pts',(0.753682061113765,1.,-2.02550428623587));
#32678=CARTESIAN_POINT('Ctrl Pts',(0.752642180488104,1.,-2.03182068456467));
#32679=CARTESIAN_POINT('Ctrl Pts',(0.751562963361383,1.,-2.03814160092173));
#32680=CARTESIAN_POINT('Ctrl Pts',(0.750444657874758,1.,-2.04446689147754));
#32681=CARTESIAN_POINT('Ctrl Pts',(0.749287468663053,1.,-2.05079645591606));
#32682=CARTESIAN_POINT('Ctrl Pts',(0.748091554181101,1.,-2.05713023030263));
#32683=CARTESIAN_POINT('Ctrl Pts',(0.747103932785504,1.,-2.06220058927162));
#32684=CARTESIAN_POINT('Ctrl Pts',(0.746345871542695,1.,-2.06600523016401));
#32685=CARTESIAN_POINT('Ctrl Pts',(0.74583279137781,1.,-2.06854248895575));
#32686=CARTESIAN_POINT('Ctrl Pts',(0.745574324794401,1.,-2.0698113262342));
#32687=CARTESIAN_POINT('',(0.693717979106306,0.,-1.60662857109684));
#32688=CARTESIAN_POINT('Origin',(0.,0.,0.));
#32689=CARTESIAN_POINT('',(0.892032620296855,1.,-1.5055822144029));
#32690=CARTESIAN_POINT('Origin',(0.,1.,0.));
#32691=CARTESIAN_POINT('',(0.892032620296855,0.,-1.5055822144029));
#32692=CARTESIAN_POINT('Ctrl Pts',(1.23627494547115,-1.,-1.81978687191668));
#32693=CARTESIAN_POINT('Ctrl Pts',(1.23627494547115,1.,-1.81978687191668));
#32694=CARTESIAN_POINT('Ctrl Pts',(1.23509651170476,-1.,-1.81925017193666));
#32695=CARTESIAN_POINT('Ctrl Pts',(1.23509651170476,1.,-1.81925017193666));
#32696=CARTESIAN_POINT('Ctrl Pts',(1.2327422452705,-1.,-1.81817389921279));
#32697=CARTESIAN_POINT('Ctrl Pts',(1.2327422452705,1.,-1.81817389921279));
#32698=CARTESIAN_POINT('Ctrl Pts',(1.2292186489137,-1.,-1.8165508718364));
#32699=CARTESIAN_POINT('Ctrl Pts',(1.2292186489137,1.,-1.8165508718364));
#32700=CARTESIAN_POINT('Ctrl Pts',(1.2245361330495,-1.,-1.81436959210434));
#32701=CARTESIAN_POINT('Ctrl Pts',(1.2245361330495,1.,-1.81436959210434));
#32702=CARTESIAN_POINT('Ctrl Pts',(1.21870906103557,-1.,-1.81161420806656));
#32703=CARTESIAN_POINT('Ctrl Pts',(1.21870906103557,1.,-1.81161420806656));
#32704=CARTESIAN_POINT('Ctrl Pts',(1.21290815708314,-1.,-1.80882996917129));
#32705=CARTESIAN_POINT('Ctrl Pts',(1.21290815708314,1.,-1.80882996917129));
#32706=CARTESIAN_POINT('Ctrl Pts',(1.20713356605475,-1.,-1.80601678480707));
#32707=CARTESIAN_POINT('Ctrl Pts',(1.20713356605475,1.,-1.80601678480707));
#32708=CARTESIAN_POINT('Ctrl Pts',(1.20138548938974,-1.,-1.80317454838603));
#32709=CARTESIAN_POINT('Ctrl Pts',(1.20138548938974,1.,-1.80317454838603));
#32710=CARTESIAN_POINT('Ctrl Pts',(1.19566418930242,-1.,-1.80030314369879));
#32711=CARTESIAN_POINT('Ctrl Pts',(1.19566418930242,1.,-1.80030314369879));
#32712=CARTESIAN_POINT('Ctrl Pts',(1.18996997934445,-1.,-1.79740245923478));
#32713=CARTESIAN_POINT('Ctrl Pts',(1.18996997934445,1.,-1.79740245923478));
#32714=CARTESIAN_POINT('Ctrl Pts',(1.18430321697432,-1.,-1.79447240321515));
#32715=CARTESIAN_POINT('Ctrl Pts',(1.18430321697432,1.,-1.79447240321515));
#32716=CARTESIAN_POINT('Ctrl Pts',(1.17866429440809,-1.,-1.79151291552689));
#32717=CARTESIAN_POINT('Ctrl Pts',(1.17866429440809,1.,-1.79151291552689));
#32718=CARTESIAN_POINT('Ctrl Pts',(1.17305363177328,-1.,-1.78852398877617));
#32719=CARTESIAN_POINT('Ctrl Pts',(1.17305363177328,1.,-1.78852398877617));
#32720=CARTESIAN_POINT('Ctrl Pts',(1.16747166312303,-1.,-1.78550566040443));
#32721=CARTESIAN_POINT('Ctrl Pts',(1.16747166312303,1.,-1.78550566040443));
#32722=CARTESIAN_POINT('Ctrl Pts',(1.16191881298499,-1.,-1.78245795881009));
#32723=CARTESIAN_POINT('Ctrl Pts',(1.16191881298499,1.,-1.78245795881009));
#32724=CARTESIAN_POINT('Ctrl Pts',(1.15639547194698,-1.,-1.77938085564275));
#32725=CARTESIAN_POINT('Ctrl Pts',(1.15639547194698,1.,-1.77938085564275));
#32726=CARTESIAN_POINT('Ctrl Pts',(1.15090197841514,-1.,-1.7762742255701));
#32727=CARTESIAN_POINT('Ctrl Pts',(1.15090197841514,1.,-1.7762742255701));
#32728=CARTESIAN_POINT('Ctrl Pts',(1.1454385822692,-1.,-1.77313777896194));
#32729=CARTESIAN_POINT('Ctrl Pts',(1.1454385822692,1.,-1.77313777896194));
#32730=CARTESIAN_POINT('Ctrl Pts',(1.14000548336975,-1.,-1.76997111386769));
#32731=CARTESIAN_POINT('Ctrl Pts',(1.14000548336975,1.,-1.76997111386769));
#32732=CARTESIAN_POINT('Ctrl Pts',(1.1346029180462,-1.,-1.76677384551862));
#32733=CARTESIAN_POINT('Ctrl Pts',(1.1346029180462,1.,-1.76677384551862));
#32734=CARTESIAN_POINT('Ctrl Pts',(1.12923123555075,-1.,-1.7635457196617));
#32735=CARTESIAN_POINT('Ctrl Pts',(1.12923123555075,1.,-1.7635457196617));
#32736=CARTESIAN_POINT('Ctrl Pts',(1.12389096855086,-1.,-1.76028671825096));
#32737=CARTESIAN_POINT('Ctrl Pts',(1.12389096855086,1.,-1.76028671825096));
#32738=CARTESIAN_POINT('Ctrl Pts',(1.11858293216763,-1.,-1.75699720772105));
#32739=CARTESIAN_POINT('Ctrl Pts',(1.11858293216763,1.,-1.75699720772105));
#32740=CARTESIAN_POINT('Ctrl Pts',(1.11330807582551,-1.,-1.7536777209463));
#32741=CARTESIAN_POINT('Ctrl Pts',(1.11330807582551,1.,-1.7536777209463));
#32742=CARTESIAN_POINT('Ctrl Pts',(1.10806728183007,-1.,-1.7503286607592));
#32743=CARTESIAN_POINT('Ctrl Pts',(1.10806728183007,1.,-1.7503286607592));
#32744=CARTESIAN_POINT('Ctrl Pts',(1.10286118991143,-1.,-1.74695004214923));
#32745=CARTESIAN_POINT('Ctrl Pts',(1.10286118991143,1.,-1.74695004214923));
#32746=CARTESIAN_POINT('Ctrl Pts',(1.09768999241225,-1.,-1.74354119236208));
#32747=CARTESIAN_POINT('Ctrl Pts',(1.09768999241225,1.,-1.74354119236208));
#32748=CARTESIAN_POINT('Ctrl Pts',(1.09255329056493,-1.,-1.74010053962247));
#32749=CARTESIAN_POINT('Ctrl Pts',(1.09255329056493,1.,-1.74010053962247));
#32750=CARTESIAN_POINT('Ctrl Pts',(1.08745056285427,-1.,-1.73662628326091));
#32751=CARTESIAN_POINT('Ctrl Pts',(1.08745056285427,1.,-1.73662628326091));
#32752=CARTESIAN_POINT('Ctrl Pts',(1.08238162784749,-1.,-1.73311705663407));
#32753=CARTESIAN_POINT('Ctrl Pts',(1.08238162784749,1.,-1.73311705663407));
#32754=CARTESIAN_POINT('Ctrl Pts',(1.0773470373727,-1.,-1.72957248977424));
#32755=CARTESIAN_POINT('Ctrl Pts',(1.0773470373727,1.,-1.72957248977424));
#32756=CARTESIAN_POINT('Ctrl Pts',(1.07234866990252,-1.,-1.72599406198488));
#32757=CARTESIAN_POINT('Ctrl Pts',(1.07234866990252,1.,-1.72599406198488));
#32758=CARTESIAN_POINT('Ctrl Pts',(1.06738966975462,-1.,-1.72238500928453));
#32759=CARTESIAN_POINT('Ctrl Pts',(1.06738966975462,1.,-1.72238500928453));
#32760=CARTESIAN_POINT('Ctrl Pts',(1.06247324680647,-1.,-1.71874858456904));
#32761=CARTESIAN_POINT('Ctrl Pts',(1.06247324680647,1.,-1.71874858456904));
#32762=CARTESIAN_POINT('Ctrl Pts',(1.05760163192479,-1.,-1.7150865442702));
#32763=CARTESIAN_POINT('Ctrl Pts',(1.05760163192479,1.,-1.7150865442702));
#32764=CARTESIAN_POINT('Ctrl Pts',(1.05277517202855,-1.,-1.71139783543989));
#32765=CARTESIAN_POINT('Ctrl Pts',(1.05277517202855,1.,-1.71139783543989));
#32766=CARTESIAN_POINT('Ctrl Pts',(1.04799085404995,-1.,-1.70767646263649));
#32767=CARTESIAN_POINT('Ctrl Pts',(1.04799085404995,1.,-1.70767646263649));
#32768=CARTESIAN_POINT('Ctrl Pts',(1.04324363334554,-1.,-1.70391338707982));
#32769=CARTESIAN_POINT('Ctrl Pts',(1.04324363334554,1.,-1.70391338707982));
#32770=CARTESIAN_POINT('Ctrl Pts',(1.03852922490789,-1.,-1.70010052930962));
#32771=CARTESIAN_POINT('Ctrl Pts',(1.03852922490789,1.,-1.70010052930962));
#32772=CARTESIAN_POINT('Ctrl Pts',(1.03384646003588,-1.,-1.69623414782771));
#32773=CARTESIAN_POINT('Ctrl Pts',(1.03384646003588,1.,-1.69623414782771));
#32774=CARTESIAN_POINT('Ctrl Pts',(1.02919977579147,-1.,-1.69231840863458));
#32775=CARTESIAN_POINT('Ctrl Pts',(1.02919977579147,1.,-1.69231840863458));
#32776=CARTESIAN_POINT('Ctrl Pts',(1.02460180535255,-1.,-1.68836910178447));
#32777=CARTESIAN_POINT('Ctrl Pts',(1.02460180535255,1.,-1.68836910178447));
#32778=CARTESIAN_POINT('Ctrl Pts',(1.02006795074201,-1.,-1.68440578021706));
#32779=CARTESIAN_POINT('Ctrl Pts',(1.02006795074201,1.,-1.68440578021706));
#32780=CARTESIAN_POINT('Ctrl Pts',(1.01561026162773,-1.,-1.68044289894798));
#32781=CARTESIAN_POINT('Ctrl Pts',(1.01561026162773,1.,-1.68044289894798));
#32782=CARTESIAN_POINT('Ctrl Pts',(1.01123236493511,-1.,-1.67648246776464));
#32783=CARTESIAN_POINT('Ctrl Pts',(1.01123236493511,1.,-1.67648246776464));
#32784=CARTESIAN_POINT('Ctrl Pts',(1.00692206696414,-1.,-1.67250335383293));
#32785=CARTESIAN_POINT('Ctrl Pts',(1.00692206696414,1.,-1.67250335383293));
#32786=CARTESIAN_POINT('Ctrl Pts',(1.00265091003727,-1.,-1.66846059277303));
#32787=CARTESIAN_POINT('Ctrl Pts',(1.00265091003727,1.,-1.66846059277303));
#32788=CARTESIAN_POINT('Ctrl Pts',(0.998389654952757,-1.,-1.66430758030376));
#32789=CARTESIAN_POINT('Ctrl Pts',(0.998389654952757,1.,-1.66430758030376));
#32790=CARTESIAN_POINT('Ctrl Pts',(0.994121836661305,-1.,-1.66001553809947));
#32791=CARTESIAN_POINT('Ctrl Pts',(0.994121836661305,1.,-1.66001553809947));
#32792=CARTESIAN_POINT('Ctrl Pts',(0.989855627854164,-1.,-1.65559044289699));
#32793=CARTESIAN_POINT('Ctrl Pts',(0.989855627854164,1.,-1.65559044289699));
#32794=CARTESIAN_POINT('Ctrl Pts',(0.98564262292082,-1.,-1.65110016612638));
#32795=CARTESIAN_POINT('Ctrl Pts',(0.98564262292082,1.,-1.65110016612638));
#32796=CARTESIAN_POINT('Ctrl Pts',(0.981562530939489,-1.,-1.64665139190656));
#32797=CARTESIAN_POINT('Ctrl Pts',(0.981562530939489,1.,-1.64665139190656));
#32798=CARTESIAN_POINT('Ctrl Pts',(0.977689794119416,-1.,-1.64233990826687));
#32799=CARTESIAN_POINT('Ctrl Pts',(0.977689794119416,1.,-1.64233990826687));
#32800=CARTESIAN_POINT('Ctrl Pts',(0.974066058287418,-1.,-1.63820952658144));
#32801=CARTESIAN_POINT('Ctrl Pts',(0.974066058287418,1.,-1.63820952658144));
#32802=CARTESIAN_POINT('Ctrl Pts',(0.970669715997509,-1.,-1.63420665729798));
#32803=CARTESIAN_POINT('Ctrl Pts',(0.970669715997509,1.,-1.63420665729798));
#32804=CARTESIAN_POINT('Ctrl Pts',(0.967387853230345,-1.,-1.63013849959462));
#32805=CARTESIAN_POINT('Ctrl Pts',(0.967387853230345,1.,-1.63013849959462));
#32806=CARTESIAN_POINT('Ctrl Pts',(0.964046107040535,-1.,-1.62571930670187));
#32807=CARTESIAN_POINT('Ctrl Pts',(0.964046107040535,1.,-1.62571930670187));
#32808=CARTESIAN_POINT('Ctrl Pts',(0.960438326101728,-1.,-1.62061638140221));
#32809=CARTESIAN_POINT('Ctrl Pts',(0.960438326101728,1.,-1.62061638140221));
#32810=CARTESIAN_POINT('Ctrl Pts',(0.95635442292067,-1.,-1.61449324337085));
#32811=CARTESIAN_POINT('Ctrl Pts',(0.95635442292067,1.,-1.61449324337085));
#32812=CARTESIAN_POINT('Ctrl Pts',(0.951613284356035,-1.,-1.60706069896936));
#32813=CARTESIAN_POINT('Ctrl Pts',(0.951613284356035,1.,-1.60706069896936));
#32814=CARTESIAN_POINT('Ctrl Pts',(0.946078063315257,-1.,-1.59810042043673));
#32815=CARTESIAN_POINT('Ctrl Pts',(0.946078063315257,1.,-1.59810042043673));
#32816=CARTESIAN_POINT('Ctrl Pts',(0.939646377893399,-1.,-1.58744937487176));
#32817=CARTESIAN_POINT('Ctrl Pts',(0.939646377893399,1.,-1.58744937487176));
#32818=CARTESIAN_POINT('Ctrl Pts',(0.932246680108685,-1.,-1.57499388382243));
#32819=CARTESIAN_POINT('Ctrl Pts',(0.932246680108685,1.,-1.57499388382243));
#32820=CARTESIAN_POINT('Ctrl Pts',(0.923832188944341,-1.,-1.56065988578893));
#32821=CARTESIAN_POINT('Ctrl Pts',(0.923832188944341,1.,-1.56065988578893));
#32822=CARTESIAN_POINT('Ctrl Pts',(0.914375919026456,-1.,-1.54440491149498));
#32823=CARTESIAN_POINT('Ctrl Pts',(0.914375919026456,1.,-1.54440491149498));
#32824=CARTESIAN_POINT('Ctrl Pts',(0.905967409625651,-1.,-1.52984849887993));
#32825=CARTESIAN_POINT('Ctrl Pts',(0.905967409625651,1.,-1.52984849887993));
#32826=CARTESIAN_POINT('Ctrl Pts',(0.89918504748351,-1.,-1.51805569590094));
#32827=CARTESIAN_POINT('Ctrl Pts',(0.89918504748351,1.,-1.51805569590094));
#32828=CARTESIAN_POINT('Ctrl Pts',(0.894452006964543,-1.,-1.50980486806688));
#32829=CARTESIAN_POINT('Ctrl Pts',(0.894452006964543,1.,-1.50980486806688));
#32830=CARTESIAN_POINT('Ctrl Pts',(0.892032620296855,-1.,-1.5055822144029));
#32831=CARTESIAN_POINT('Ctrl Pts',(0.892032620296855,1.,-1.5055822144029));
#32832=CARTESIAN_POINT('',(1.23627494547115,1.,-1.81978687191668));
#32833=CARTESIAN_POINT('Ctrl Pts',(1.23627494547115,1.,-1.81978687191668));
#32834=CARTESIAN_POINT('Ctrl Pts',(1.23509651170476,1.,-1.81925017193666));
#32835=CARTESIAN_POINT('Ctrl Pts',(1.2327422452705,1.,-1.81817389921279));
#32836=CARTESIAN_POINT('Ctrl Pts',(1.2292186489137,1.,-1.8165508718364));
#32837=CARTESIAN_POINT('Ctrl Pts',(1.2245361330495,1.,-1.81436959210434));
#32838=CARTESIAN_POINT('Ctrl Pts',(1.21870906103557,1.,-1.81161420806656));
#32839=CARTESIAN_POINT('Ctrl Pts',(1.21290815708314,1.,-1.80882996917129));
#32840=CARTESIAN_POINT('Ctrl Pts',(1.20713356605475,1.,-1.80601678480707));
#32841=CARTESIAN_POINT('Ctrl Pts',(1.20138548938974,1.,-1.80317454838603));
#32842=CARTESIAN_POINT('Ctrl Pts',(1.19566418930242,1.,-1.80030314369879));
#32843=CARTESIAN_POINT('Ctrl Pts',(1.18996997934445,1.,-1.79740245923478));
#32844=CARTESIAN_POINT('Ctrl Pts',(1.18430321697432,1.,-1.79447240321515));
#32845=CARTESIAN_POINT('Ctrl Pts',(1.17866429440809,1.,-1.79151291552689));
#32846=CARTESIAN_POINT('Ctrl Pts',(1.17305363177328,1.,-1.78852398877617));
#32847=CARTESIAN_POINT('Ctrl Pts',(1.16747166312303,1.,-1.78550566040443));
#32848=CARTESIAN_POINT('Ctrl Pts',(1.16191881298499,1.,-1.78245795881009));
#32849=CARTESIAN_POINT('Ctrl Pts',(1.15639547194698,1.,-1.77938085564275));
#32850=CARTESIAN_POINT('Ctrl Pts',(1.15090197841514,1.,-1.7762742255701));
#32851=CARTESIAN_POINT('Ctrl Pts',(1.1454385822692,1.,-1.77313777896194));
#32852=CARTESIAN_POINT('Ctrl Pts',(1.14000548336975,1.,-1.76997111386769));
#32853=CARTESIAN_POINT('Ctrl Pts',(1.1346029180462,1.,-1.76677384551862));
#32854=CARTESIAN_POINT('Ctrl Pts',(1.12923123555075,1.,-1.7635457196617));
#32855=CARTESIAN_POINT('Ctrl Pts',(1.12389096855086,1.,-1.76028671825096));
#32856=CARTESIAN_POINT('Ctrl Pts',(1.11858293216763,1.,-1.75699720772105));
#32857=CARTESIAN_POINT('Ctrl Pts',(1.11330807582551,1.,-1.7536777209463));
#32858=CARTESIAN_POINT('Ctrl Pts',(1.10806728183007,1.,-1.7503286607592));
#32859=CARTESIAN_POINT('Ctrl Pts',(1.10286118991143,1.,-1.74695004214923));
#32860=CARTESIAN_POINT('Ctrl Pts',(1.09768999241225,1.,-1.74354119236208));
#32861=CARTESIAN_POINT('Ctrl Pts',(1.09255329056493,1.,-1.74010053962247));
#32862=CARTESIAN_POINT('Ctrl Pts',(1.08745056285427,1.,-1.73662628326091));
#32863=CARTESIAN_POINT('Ctrl Pts',(1.08238162784749,1.,-1.73311705663407));
#32864=CARTESIAN_POINT('Ctrl Pts',(1.0773470373727,1.,-1.72957248977424));
#32865=CARTESIAN_POINT('Ctrl Pts',(1.07234866990252,1.,-1.72599406198488));
#32866=CARTESIAN_POINT('Ctrl Pts',(1.06738966975462,1.,-1.72238500928453));
#32867=CARTESIAN_POINT('Ctrl Pts',(1.06247324680647,1.,-1.71874858456904));
#32868=CARTESIAN_POINT('Ctrl Pts',(1.05760163192479,1.,-1.7150865442702));
#32869=CARTESIAN_POINT('Ctrl Pts',(1.05277517202855,1.,-1.71139783543989));
#32870=CARTESIAN_POINT('Ctrl Pts',(1.04799085404995,1.,-1.70767646263649));
#32871=CARTESIAN_POINT('Ctrl Pts',(1.04324363334554,1.,-1.70391338707982));
#32872=CARTESIAN_POINT('Ctrl Pts',(1.03852922490789,1.,-1.70010052930962));
#32873=CARTESIAN_POINT('Ctrl Pts',(1.03384646003588,1.,-1.69623414782771));
#32874=CARTESIAN_POINT('Ctrl Pts',(1.02919977579147,1.,-1.69231840863458));
#32875=CARTESIAN_POINT('Ctrl Pts',(1.02460180535255,1.,-1.68836910178447));
#32876=CARTESIAN_POINT('Ctrl Pts',(1.02006795074201,1.,-1.68440578021706));
#32877=CARTESIAN_POINT('Ctrl Pts',(1.01561026162773,1.,-1.68044289894798));
#32878=CARTESIAN_POINT('Ctrl Pts',(1.01123236493511,1.,-1.67648246776464));
#32879=CARTESIAN_POINT('Ctrl Pts',(1.00692206696414,1.,-1.67250335383293));
#32880=CARTESIAN_POINT('Ctrl Pts',(1.00265091003727,1.,-1.66846059277303));
#32881=CARTESIAN_POINT('Ctrl Pts',(0.998389654952757,1.,-1.66430758030376));
#32882=CARTESIAN_POINT('Ctrl Pts',(0.994121836661305,1.,-1.66001553809947));
#32883=CARTESIAN_POINT('Ctrl Pts',(0.989855627854164,1.,-1.65559044289699));
#32884=CARTESIAN_POINT('Ctrl Pts',(0.98564262292082,1.,-1.65110016612638));
#32885=CARTESIAN_POINT('Ctrl Pts',(0.981562530939489,1.,-1.64665139190656));
#32886=CARTESIAN_POINT('Ctrl Pts',(0.977689794119416,1.,-1.64233990826687));
#32887=CARTESIAN_POINT('Ctrl Pts',(0.974066058287418,1.,-1.63820952658144));
#32888=CARTESIAN_POINT('Ctrl Pts',(0.970669715997509,1.,-1.63420665729798));
#32889=CARTESIAN_POINT('Ctrl Pts',(0.967387853230345,1.,-1.63013849959462));
#32890=CARTESIAN_POINT('Ctrl Pts',(0.964046107040535,1.,-1.62571930670187));
#32891=CARTESIAN_POINT('Ctrl Pts',(0.960438326101728,1.,-1.62061638140221));
#32892=CARTESIAN_POINT('Ctrl Pts',(0.95635442292067,1.,-1.61449324337085));
#32893=CARTESIAN_POINT('Ctrl Pts',(0.951613284356035,1.,-1.60706069896936));
#32894=CARTESIAN_POINT('Ctrl Pts',(0.946078063315257,1.,-1.59810042043673));
#32895=CARTESIAN_POINT('Ctrl Pts',(0.939646377893399,1.,-1.58744937487176));
#32896=CARTESIAN_POINT('Ctrl Pts',(0.932246680108685,1.,-1.57499388382243));
#32897=CARTESIAN_POINT('Ctrl Pts',(0.923832188944341,1.,-1.56065988578893));
#32898=CARTESIAN_POINT('Ctrl Pts',(0.914375919026456,1.,-1.54440491149498));
#32899=CARTESIAN_POINT('Ctrl Pts',(0.905967409625651,1.,-1.52984849887993));
#32900=CARTESIAN_POINT('Ctrl Pts',(0.89918504748351,1.,-1.51805569590094));
#32901=CARTESIAN_POINT('Ctrl Pts',(0.894452006964543,1.,-1.50980486806688));
#32902=CARTESIAN_POINT('Ctrl Pts',(0.892032620296855,1.,-1.5055822144029));
#32903=CARTESIAN_POINT('',(1.23627494547115,0.,-1.81978687191668));
#32904=CARTESIAN_POINT('Origin',(1.34869019493419,0.,-1.73811241238545));
#32905=CARTESIAN_POINT('',(1.34869019493419,1.,-1.73811241238545));
#32906=CARTESIAN_POINT('',(1.23627494547115,1.,-1.81978687191668));
#32907=CARTESIAN_POINT('',(1.34869019493419,0.,-1.73811241238545));
#32908=CARTESIAN_POINT('Ctrl Pts',(1.15624053661742,-1.,-1.31362392696032));
#32909=CARTESIAN_POINT('Ctrl Pts',(1.15624053661742,1.,-1.31362392696032));
#32910=CARTESIAN_POINT('Ctrl Pts',(1.15950888730809,-1.,-1.31722977216397));
#32911=CARTESIAN_POINT('Ctrl Pts',(1.15950888730809,1.,-1.31722977216397));
#32912=CARTESIAN_POINT('Ctrl Pts',(1.16589330093588,-1.,-1.32428080721772));
#32913=CARTESIAN_POINT('Ctrl Pts',(1.16589330093588,1.,-1.32428080721772));
#32914=CARTESIAN_POINT('Ctrl Pts',(1.17501305789857,-1.,-1.33437539347008));
#32915=CARTESIAN_POINT('Ctrl Pts',(1.17501305789857,1.,-1.33437539347008));
#32916=CARTESIAN_POINT('Ctrl Pts',(1.18625865667441,-1.,-1.34687054001093));
#32917=CARTESIAN_POINT('Ctrl Pts',(1.18625865667441,1.,-1.34687054001093));
#32918=CARTESIAN_POINT('Ctrl Pts',(1.1987959077932,-1.,-1.36088705043885));
#32919=CARTESIAN_POINT('Ctrl Pts',(1.1987959077932,1.,-1.36088705043885));
#32920=CARTESIAN_POINT('Ctrl Pts',(1.20982812925645,-1.,-1.37331915607905));
#32921=CARTESIAN_POINT('Ctrl Pts',(1.20982812925645,1.,-1.37331915607905));
#32922=CARTESIAN_POINT('Ctrl Pts',(1.21938737280852,-1.,-1.38420564527715));
#32923=CARTESIAN_POINT('Ctrl Pts',(1.21938737280852,1.,-1.38420564527715));
#32924=CARTESIAN_POINT('Ctrl Pts',(1.22752961899387,-1.,-1.39361389568796));
#32925=CARTESIAN_POINT('Ctrl Pts',(1.22752961899387,1.,-1.39361389568796));
#32926=CARTESIAN_POINT('Ctrl Pts',(1.23434087290423,-1.,-1.40164708206106));
#32927=CARTESIAN_POINT('Ctrl Pts',(1.23434087290423,1.,-1.40164708206106));
#32928=CARTESIAN_POINT('Ctrl Pts',(1.23994455029534,-1.,-1.40845295531283));
#32929=CARTESIAN_POINT('Ctrl Pts',(1.23994455029534,1.,-1.40845295531283));
#32930=CARTESIAN_POINT('Ctrl Pts',(1.24450600513056,-1.,-1.41422913175179));
#32931=CARTESIAN_POINT('Ctrl Pts',(1.24450600513056,1.,-1.41422913175179));
#32932=CARTESIAN_POINT('Ctrl Pts',(1.24824430986571,-1.,-1.41923722596025));
#32933=CARTESIAN_POINT('Ctrl Pts',(1.24824430986571,1.,-1.41923722596025));
#32934=CARTESIAN_POINT('Ctrl Pts',(1.2514145557001,-1.,-1.42378102115575));
#32935=CARTESIAN_POINT('Ctrl Pts',(1.2514145557001,1.,-1.42378102115575));
#32936=CARTESIAN_POINT('Ctrl Pts',(1.25426945222639,-1.,-1.42815938799387));
#32937=CARTESIAN_POINT('Ctrl Pts',(1.25426945222639,1.,-1.42815938799387));
#32938=CARTESIAN_POINT('Ctrl Pts',(1.25702687965755,-1.,-1.43262645609691));
#32939=CARTESIAN_POINT('Ctrl Pts',(1.25702687965755,1.,-1.43262645609691));
#32940=CARTESIAN_POINT('Ctrl Pts',(1.25983531012005,-1.,-1.43734919180848));
#32941=CARTESIAN_POINT('Ctrl Pts',(1.25983531012005,1.,-1.43734919180848));
#32942=CARTESIAN_POINT('Ctrl Pts',(1.26273903323858,-1.,-1.44236470511303));
#32943=CARTESIAN_POINT('Ctrl Pts',(1.26273903323858,1.,-1.44236470511303));
#32944=CARTESIAN_POINT('Ctrl Pts',(1.26570925118868,-1.,-1.44761985001662));
#32945=CARTESIAN_POINT('Ctrl Pts',(1.26570925118868,1.,-1.44761985001662));
#32946=CARTESIAN_POINT('Ctrl Pts',(1.2686778680489,-1.,-1.45301422764247));
#32947=CARTESIAN_POINT('Ctrl Pts',(1.2686778680489,1.,-1.45301422764247));
#32948=CARTESIAN_POINT('Ctrl Pts',(1.27156805265289,-1.,-1.45843906294697));
#32949=CARTESIAN_POINT('Ctrl Pts',(1.27156805265289,1.,-1.45843906294697));
#32950=CARTESIAN_POINT('Ctrl Pts',(1.27433119897822,-1.,-1.46382431332476));
#32951=CARTESIAN_POINT('Ctrl Pts',(1.27433119897822,1.,-1.46382431332476));
#32952=CARTESIAN_POINT('Ctrl Pts',(1.27696414831089,-1.,-1.46916035917133));
#32953=CARTESIAN_POINT('Ctrl Pts',(1.27696414831089,1.,-1.46916035917133));
#32954=CARTESIAN_POINT('Ctrl Pts',(1.2794891824849,-1.,-1.4744717526707));
#32955=CARTESIAN_POINT('Ctrl Pts',(1.2794891824849,1.,-1.4744717526707));
#32956=CARTESIAN_POINT('Ctrl Pts',(1.28194158939517,-1.,-1.47980070347096));
#32957=CARTESIAN_POINT('Ctrl Pts',(1.28194158939517,1.,-1.47980070347096));
#32958=CARTESIAN_POINT('Ctrl Pts',(1.28435533880201,-1.,-1.4851881711891));
#32959=CARTESIAN_POINT('Ctrl Pts',(1.28435533880201,1.,-1.4851881711891));
#32960=CARTESIAN_POINT('Ctrl Pts',(1.2867467611644,-1.,-1.4906522831278));
#32961=CARTESIAN_POINT('Ctrl Pts',(1.2867467611644,1.,-1.4906522831278));
#32962=CARTESIAN_POINT('Ctrl Pts',(1.28911506584254,-1.,-1.49618896881754));
#32963=CARTESIAN_POINT('Ctrl Pts',(1.28911506584254,1.,-1.49618896881754));
#32964=CARTESIAN_POINT('Ctrl Pts',(1.29145022885181,-1.,-1.50178230149776));
#32965=CARTESIAN_POINT('Ctrl Pts',(1.29145022885181,1.,-1.50178230149776));
#32966=CARTESIAN_POINT('Ctrl Pts',(1.29373841372842,-1.,-1.50741159078365));
#32967=CARTESIAN_POINT('Ctrl Pts',(1.29373841372842,1.,-1.50741159078365));
#32968=CARTESIAN_POINT('Ctrl Pts',(1.29596850710509,-1.,-1.51305994241402));
#32969=CARTESIAN_POINT('Ctrl Pts',(1.29596850710509,1.,-1.51305994241402));
#32970=CARTESIAN_POINT('Ctrl Pts',(1.29813791800747,-1.,-1.51872184912724));
#32971=CARTESIAN_POINT('Ctrl Pts',(1.29813791800747,1.,-1.51872184912724));
#32972=CARTESIAN_POINT('Ctrl Pts',(1.30024984366328,-1.,-1.52439957861062));
#32973=CARTESIAN_POINT('Ctrl Pts',(1.30024984366328,1.,-1.52439957861062));
#32974=CARTESIAN_POINT('Ctrl Pts',(1.30231064395568,-1.,-1.53009970283891));
#32975=CARTESIAN_POINT('Ctrl Pts',(1.30231064395568,1.,-1.53009970283891));
#32976=CARTESIAN_POINT('Ctrl Pts',(1.30432735639489,-1.,-1.53582981268977));
#32977=CARTESIAN_POINT('Ctrl Pts',(1.30432735639489,1.,-1.53582981268977));
#32978=CARTESIAN_POINT('Ctrl Pts',(1.30630475189556,-1.,-1.54159462645432));
#32979=CARTESIAN_POINT('Ctrl Pts',(1.30630475189556,1.,-1.54159462645432));
#32980=CARTESIAN_POINT('Ctrl Pts',(1.30824393907473,-1.,-1.54739413957185));
#32981=CARTESIAN_POINT('Ctrl Pts',(1.30824393907473,1.,-1.54739413957185));
#32982=CARTESIAN_POINT('Ctrl Pts',(1.31014393684222,-1.,-1.55322568759481));
#32983=CARTESIAN_POINT('Ctrl Pts',(1.31014393684222,1.,-1.55322568759481));
#32984=CARTESIAN_POINT('Ctrl Pts',(1.31200264341696,-1.,-1.55908521254821));
#32985=CARTESIAN_POINT('Ctrl Pts',(1.31200264341696,1.,-1.55908521254821));
#32986=CARTESIAN_POINT('Ctrl Pts',(1.31381795281002,-1.,-1.56496872402353));
#32987=CARTESIAN_POINT('Ctrl Pts',(1.31381795281002,1.,-1.56496872402353));
#32988=CARTESIAN_POINT('Ctrl Pts',(1.31558903860016,-1.,-1.57087397835723));
#32989=CARTESIAN_POINT('Ctrl Pts',(1.31558903860016,1.,-1.57087397835723));
#32990=CARTESIAN_POINT('Ctrl Pts',(1.31731642317187,-1.,-1.5768005650559));
#32991=CARTESIAN_POINT('Ctrl Pts',(1.31731642317187,1.,-1.5768005650559));
#32992=CARTESIAN_POINT('Ctrl Pts',(1.31900135021432,-1.,-1.58274907898834));
#32993=CARTESIAN_POINT('Ctrl Pts',(1.31900135021432,1.,-1.58274907898834));
#32994=CARTESIAN_POINT('Ctrl Pts',(1.32064537110892,-1.,-1.58872057258245));
#32995=CARTESIAN_POINT('Ctrl Pts',(1.32064537110892,1.,-1.58872057258245));
#32996=CARTESIAN_POINT('Ctrl Pts',(1.32224985747682,-1.,-1.59471591079403));
#32997=CARTESIAN_POINT('Ctrl Pts',(1.32224985747682,1.,-1.59471591079403));
#32998=CARTESIAN_POINT('Ctrl Pts',(1.32381550858256,-1.,-1.60073511858687));
#32999=CARTESIAN_POINT('Ctrl Pts',(1.32381550858256,1.,-1.60073511858687));
#33000=CARTESIAN_POINT('Ctrl Pts',(1.32534250785782,-1.,-1.60677758290954));
#33001=CARTESIAN_POINT('Ctrl Pts',(1.32534250785782,1.,-1.60677758290954));
#33002=CARTESIAN_POINT('Ctrl Pts',(1.32683074483356,-1.,-1.6128423401575));
#33003=CARTESIAN_POINT('Ctrl Pts',(1.32683074483356,1.,-1.6128423401575));
#33004=CARTESIAN_POINT('Ctrl Pts',(1.32828000610449,-1.,-1.61892832270724));
#33005=CARTESIAN_POINT('Ctrl Pts',(1.32828000610449,1.,-1.61892832270724));
#33006=CARTESIAN_POINT('Ctrl Pts',(1.3296901950568,-1.,-1.62503464209797));
#33007=CARTESIAN_POINT('Ctrl Pts',(1.3296901950568,1.,-1.62503464209797));
#33008=CARTESIAN_POINT('Ctrl Pts',(1.33106149345645,-1.,-1.63116079730923));
#33009=CARTESIAN_POINT('Ctrl Pts',(1.33106149345645,1.,-1.63116079730923));
#33010=CARTESIAN_POINT('Ctrl Pts',(1.33239425103724,-1.,-1.63730653475089));
#33011=CARTESIAN_POINT('Ctrl Pts',(1.33239425103724,1.,-1.63730653475089));
#33012=CARTESIAN_POINT('Ctrl Pts',(1.33368890676572,-1.,-1.6434717485603));
#33013=CARTESIAN_POINT('Ctrl Pts',(1.33368890676572,1.,-1.6434717485603));
#33014=CARTESIAN_POINT('Ctrl Pts',(1.33494590467993,-1.,-1.6496563728683));
#33015=CARTESIAN_POINT('Ctrl Pts',(1.33494590467993,1.,-1.6496563728683));
#33016=CARTESIAN_POINT('Ctrl Pts',(1.33616559745172,-1.,-1.65586025952593));
#33017=CARTESIAN_POINT('Ctrl Pts',(1.33616559745172,1.,-1.65586025952593));
#33018=CARTESIAN_POINT('Ctrl Pts',(1.33734820885262,-1.,-1.66208312541983));
#33019=CARTESIAN_POINT('Ctrl Pts',(1.33734820885262,1.,-1.66208312541983));
#33020=CARTESIAN_POINT('Ctrl Pts',(1.33849388654388,-1.,-1.66832460783989));
#33021=CARTESIAN_POINT('Ctrl Pts',(1.33849388654388,1.,-1.66832460783989));
#33022=CARTESIAN_POINT('Ctrl Pts',(1.3396027347034,-1.,-1.67458429426086));
#33023=CARTESIAN_POINT('Ctrl Pts',(1.3396027347034,1.,-1.67458429426086));
#33024=CARTESIAN_POINT('Ctrl Pts',(1.34067485185203,-1.,-1.68086176030362));
#33025=CARTESIAN_POINT('Ctrl Pts',(1.34067485185203,1.,-1.68086176030362));
#33026=CARTESIAN_POINT('Ctrl Pts',(1.341710374848,-1.,-1.68715660868764));
#33027=CARTESIAN_POINT('Ctrl Pts',(1.341710374848,1.,-1.68715660868764));
#33028=CARTESIAN_POINT('Ctrl Pts',(1.34270948206319,-1.,-1.6934684849687));
#33029=CARTESIAN_POINT('Ctrl Pts',(1.34270948206319,1.,-1.6934684849687));
#33030=CARTESIAN_POINT('Ctrl Pts',(1.34367237124483,-1.,-1.69979707754427));
#33031=CARTESIAN_POINT('Ctrl Pts',(1.34367237124483,1.,-1.69979707754427));
#33032=CARTESIAN_POINT('Ctrl Pts',(1.34459924533831,-1.,-1.70614212266738));
#33033=CARTESIAN_POINT('Ctrl Pts',(1.34459924533831,1.,-1.70614212266738));
#33034=CARTESIAN_POINT('Ctrl Pts',(1.34549029589416,-1.,-1.71250340686822));
#33035=CARTESIAN_POINT('Ctrl Pts',(1.34549029589416,1.,-1.71250340686822));
#33036=CARTESIAN_POINT('Ctrl Pts',(1.34634568653227,-1.,-1.7188807715049));
#33037=CARTESIAN_POINT('Ctrl Pts',(1.34634568653227,1.,-1.7188807715049));
#33038=CARTESIAN_POINT('Ctrl Pts',(1.34716554819527,-1.,-1.72527410680674));
#33039=CARTESIAN_POINT('Ctrl Pts',(1.34716554819527,1.,-1.72527410680674));
#33040=CARTESIAN_POINT('Ctrl Pts',(1.34779309152035,-1.,-1.7304014965394));
#33041=CARTESIAN_POINT('Ctrl Pts',(1.34779309152035,1.,-1.7304014965394));
#33042=CARTESIAN_POINT('Ctrl Pts',(1.34824783112887,-1.,-1.73425417885907));
#33043=CARTESIAN_POINT('Ctrl Pts',(1.34824783112887,1.,-1.73425417885907));
#33044=CARTESIAN_POINT('Ctrl Pts',(1.34854391898045,-1.,-1.73682580585691));
#33045=CARTESIAN_POINT('Ctrl Pts',(1.34854391898045,1.,-1.73682580585691));
#33046=CARTESIAN_POINT('Ctrl Pts',(1.34869019493419,-1.,-1.73811241238545));
#33047=CARTESIAN_POINT('Ctrl Pts',(1.34869019493419,1.,-1.73811241238545));
#33048=CARTESIAN_POINT('',(1.15624053661742,1.,-1.31362392696032));
#33049=CARTESIAN_POINT('Ctrl Pts',(1.15624053661742,1.,-1.31362392696032));
#33050=CARTESIAN_POINT('Ctrl Pts',(1.15950888730809,1.,-1.31722977216397));
#33051=CARTESIAN_POINT('Ctrl Pts',(1.16589330093588,1.,-1.32428080721772));
#33052=CARTESIAN_POINT('Ctrl Pts',(1.17501305789857,1.,-1.33437539347008));
#33053=CARTESIAN_POINT('Ctrl Pts',(1.18625865667441,1.,-1.34687054001093));
#33054=CARTESIAN_POINT('Ctrl Pts',(1.1987959077932,1.,-1.36088705043885));
#33055=CARTESIAN_POINT('Ctrl Pts',(1.20982812925645,1.,-1.37331915607905));
#33056=CARTESIAN_POINT('Ctrl Pts',(1.21938737280852,1.,-1.38420564527715));
#33057=CARTESIAN_POINT('Ctrl Pts',(1.22752961899387,1.,-1.39361389568796));
#33058=CARTESIAN_POINT('Ctrl Pts',(1.23434087290423,1.,-1.40164708206106));
#33059=CARTESIAN_POINT('Ctrl Pts',(1.23994455029534,1.,-1.40845295531283));
#33060=CARTESIAN_POINT('Ctrl Pts',(1.24450600513056,1.,-1.41422913175179));
#33061=CARTESIAN_POINT('Ctrl Pts',(1.24824430986571,1.,-1.41923722596025));
#33062=CARTESIAN_POINT('Ctrl Pts',(1.2514145557001,1.,-1.42378102115575));
#33063=CARTESIAN_POINT('Ctrl Pts',(1.25426945222639,1.,-1.42815938799387));
#33064=CARTESIAN_POINT('Ctrl Pts',(1.25702687965755,1.,-1.43262645609691));
#33065=CARTESIAN_POINT('Ctrl Pts',(1.25983531012005,1.,-1.43734919180848));
#33066=CARTESIAN_POINT('Ctrl Pts',(1.26273903323858,1.,-1.44236470511303));
#33067=CARTESIAN_POINT('Ctrl Pts',(1.26570925118868,1.,-1.44761985001662));
#33068=CARTESIAN_POINT('Ctrl Pts',(1.2686778680489,1.,-1.45301422764247));
#33069=CARTESIAN_POINT('Ctrl Pts',(1.27156805265289,1.,-1.45843906294697));
#33070=CARTESIAN_POINT('Ctrl Pts',(1.27433119897822,1.,-1.46382431332476));
#33071=CARTESIAN_POINT('Ctrl Pts',(1.27696414831089,1.,-1.46916035917133));
#33072=CARTESIAN_POINT('Ctrl Pts',(1.2794891824849,1.,-1.4744717526707));
#33073=CARTESIAN_POINT('Ctrl Pts',(1.28194158939517,1.,-1.47980070347096));
#33074=CARTESIAN_POINT('Ctrl Pts',(1.28435533880201,1.,-1.4851881711891));
#33075=CARTESIAN_POINT('Ctrl Pts',(1.2867467611644,1.,-1.4906522831278));
#33076=CARTESIAN_POINT('Ctrl Pts',(1.28911506584254,1.,-1.49618896881754));
#33077=CARTESIAN_POINT('Ctrl Pts',(1.29145022885181,1.,-1.50178230149776));
#33078=CARTESIAN_POINT('Ctrl Pts',(1.29373841372842,1.,-1.50741159078365));
#33079=CARTESIAN_POINT('Ctrl Pts',(1.29596850710509,1.,-1.51305994241402));
#33080=CARTESIAN_POINT('Ctrl Pts',(1.29813791800747,1.,-1.51872184912724));
#33081=CARTESIAN_POINT('Ctrl Pts',(1.30024984366328,1.,-1.52439957861062));
#33082=CARTESIAN_POINT('Ctrl Pts',(1.30231064395568,1.,-1.53009970283891));
#33083=CARTESIAN_POINT('Ctrl Pts',(1.30432735639489,1.,-1.53582981268977));
#33084=CARTESIAN_POINT('Ctrl Pts',(1.30630475189556,1.,-1.54159462645432));
#33085=CARTESIAN_POINT('Ctrl Pts',(1.30824393907473,1.,-1.54739413957185));
#33086=CARTESIAN_POINT('Ctrl Pts',(1.31014393684222,1.,-1.55322568759481));
#33087=CARTESIAN_POINT('Ctrl Pts',(1.31200264341696,1.,-1.55908521254821));
#33088=CARTESIAN_POINT('Ctrl Pts',(1.31381795281002,1.,-1.56496872402353));
#33089=CARTESIAN_POINT('Ctrl Pts',(1.31558903860016,1.,-1.57087397835723));
#33090=CARTESIAN_POINT('Ctrl Pts',(1.31731642317187,1.,-1.5768005650559));
#33091=CARTESIAN_POINT('Ctrl Pts',(1.31900135021432,1.,-1.58274907898834));
#33092=CARTESIAN_POINT('Ctrl Pts',(1.32064537110892,1.,-1.58872057258245));
#33093=CARTESIAN_POINT('Ctrl Pts',(1.32224985747682,1.,-1.59471591079403));
#33094=CARTESIAN_POINT('Ctrl Pts',(1.32381550858256,1.,-1.60073511858687));
#33095=CARTESIAN_POINT('Ctrl Pts',(1.32534250785782,1.,-1.60677758290954));
#33096=CARTESIAN_POINT('Ctrl Pts',(1.32683074483356,1.,-1.6128423401575));
#33097=CARTESIAN_POINT('Ctrl Pts',(1.32828000610449,1.,-1.61892832270724));
#33098=CARTESIAN_POINT('Ctrl Pts',(1.3296901950568,1.,-1.62503464209797));
#33099=CARTESIAN_POINT('Ctrl Pts',(1.33106149345645,1.,-1.63116079730923));
#33100=CARTESIAN_POINT('Ctrl Pts',(1.33239425103724,1.,-1.63730653475089));
#33101=CARTESIAN_POINT('Ctrl Pts',(1.33368890676572,1.,-1.6434717485603));
#33102=CARTESIAN_POINT('Ctrl Pts',(1.33494590467993,1.,-1.6496563728683));
#33103=CARTESIAN_POINT('Ctrl Pts',(1.33616559745172,1.,-1.65586025952593));
#33104=CARTESIAN_POINT('Ctrl Pts',(1.33734820885262,1.,-1.66208312541983));
#33105=CARTESIAN_POINT('Ctrl Pts',(1.33849388654388,1.,-1.66832460783989));
#33106=CARTESIAN_POINT('Ctrl Pts',(1.3396027347034,1.,-1.67458429426086));
#33107=CARTESIAN_POINT('Ctrl Pts',(1.34067485185203,1.,-1.68086176030362));
#33108=CARTESIAN_POINT('Ctrl Pts',(1.341710374848,1.,-1.68715660868764));
#33109=CARTESIAN_POINT('Ctrl Pts',(1.34270948206319,1.,-1.6934684849687));
#33110=CARTESIAN_POINT('Ctrl Pts',(1.34367237124483,1.,-1.69979707754427));
#33111=CARTESIAN_POINT('Ctrl Pts',(1.34459924533831,1.,-1.70614212266738));
#33112=CARTESIAN_POINT('Ctrl Pts',(1.34549029589416,1.,-1.71250340686822));
#33113=CARTESIAN_POINT('Ctrl Pts',(1.34634568653227,1.,-1.7188807715049));
#33114=CARTESIAN_POINT('Ctrl Pts',(1.34716554819527,1.,-1.72527410680674));
#33115=CARTESIAN_POINT('Ctrl Pts',(1.34779309152035,1.,-1.7304014965394));
#33116=CARTESIAN_POINT('Ctrl Pts',(1.34824783112887,1.,-1.73425417885907));
#33117=CARTESIAN_POINT('Ctrl Pts',(1.34854391898045,1.,-1.73682580585691));
#33118=CARTESIAN_POINT('Ctrl Pts',(1.34869019493419,1.,-1.73811241238545));
#33119=CARTESIAN_POINT('',(1.15624053661742,0.,-1.31362392696032));
#33120=CARTESIAN_POINT('Origin',(0.,0.,0.));
#33121=CARTESIAN_POINT('',(1.31362392696032,1.,-1.15624053661742));
#33122=CARTESIAN_POINT('Origin',(0.,1.,0.));
#33123=CARTESIAN_POINT('',(1.31362392696032,0.,-1.15624053661742));
#33124=CARTESIAN_POINT('Ctrl Pts',(1.73811241238545,-1.,-1.34869019493419));
#33125=CARTESIAN_POINT('Ctrl Pts',(1.73811241238545,1.,-1.34869019493419));
#33126=CARTESIAN_POINT('Ctrl Pts',(1.73682580585819,-1.,-1.34854391898145));
#33127=CARTESIAN_POINT('Ctrl Pts',(1.73682580585819,1.,-1.34854391898145));
#33128=CARTESIAN_POINT('Ctrl Pts',(1.73425417886254,-1.,-1.34824783113158));
#33129=CARTESIAN_POINT('Ctrl Pts',(1.73425417886254,1.,-1.34824783113158));
#33130=CARTESIAN_POINT('Ctrl Pts',(1.73040149654497,-1.,-1.3477930915247));
#33131=CARTESIAN_POINT('Ctrl Pts',(1.73040149654497,1.,-1.3477930915247));
#33132=CARTESIAN_POINT('Ctrl Pts',(1.72527410681298,-1.,-1.34716554820013));
#33133=CARTESIAN_POINT('Ctrl Pts',(1.72527410681298,1.,-1.34716554820013));
#33134=CARTESIAN_POINT('Ctrl Pts',(1.7188807715095,-1.,-1.34634568653586));
#33135=CARTESIAN_POINT('Ctrl Pts',(1.7188807715095,1.,-1.34634568653586));
#33136=CARTESIAN_POINT('Ctrl Pts',(1.71250340687011,-1.,-1.34549029589563));
#33137=CARTESIAN_POINT('Ctrl Pts',(1.71250340687011,1.,-1.34549029589563));
#33138=CARTESIAN_POINT('Ctrl Pts',(1.70614212266676,-1.,-1.34459924533783));
#33139=CARTESIAN_POINT('Ctrl Pts',(1.70614212266676,1.,-1.34459924533783));
#33140=CARTESIAN_POINT('Ctrl Pts',(1.69979707754221,-1.,-1.34367237124322));
#33141=CARTESIAN_POINT('Ctrl Pts',(1.69979707754221,1.,-1.34367237124322));
#33142=CARTESIAN_POINT('Ctrl Pts',(1.6934684849664,-1.,-1.34270948206139));
#33143=CARTESIAN_POINT('Ctrl Pts',(1.6934684849664,1.,-1.34270948206139));
#33144=CARTESIAN_POINT('Ctrl Pts',(1.68715660868602,-1.,-1.34171037484673));
#33145=CARTESIAN_POINT('Ctrl Pts',(1.68715660868602,1.,-1.34171037484673));
#33146=CARTESIAN_POINT('Ctrl Pts',(1.68086176030308,-1.,-1.3406748518516));
#33147=CARTESIAN_POINT('Ctrl Pts',(1.68086176030308,1.,-1.3406748518516));
#33148=CARTESIAN_POINT('Ctrl Pts',(1.67458429426126,-1.,-1.33960273470372));
#33149=CARTESIAN_POINT('Ctrl Pts',(1.67458429426126,1.,-1.33960273470372));
#33150=CARTESIAN_POINT('Ctrl Pts',(1.66832460784078,-1.,-1.33849388654458));
#33151=CARTESIAN_POINT('Ctrl Pts',(1.66832460784078,1.,-1.33849388654458));
#33152=CARTESIAN_POINT('Ctrl Pts',(1.66208312542073,-1.,-1.33734820885331));
#33153=CARTESIAN_POINT('Ctrl Pts',(1.66208312542073,1.,-1.33734820885331));
#33154=CARTESIAN_POINT('Ctrl Pts',(1.65586025952651,-1.,-1.33616559745217));
#33155=CARTESIAN_POINT('Ctrl Pts',(1.65586025952651,1.,-1.33616559745217));
#33156=CARTESIAN_POINT('Ctrl Pts',(1.64965637286843,-1.,-1.33494590468003));
#33157=CARTESIAN_POINT('Ctrl Pts',(1.64965637286843,1.,-1.33494590468003));
#33158=CARTESIAN_POINT('Ctrl Pts',(1.64347174856007,-1.,-1.33368890676554));
#33159=CARTESIAN_POINT('Ctrl Pts',(1.64347174856007,1.,-1.33368890676554));
#33160=CARTESIAN_POINT('Ctrl Pts',(1.63730653475049,-1.,-1.33239425103694));
#33161=CARTESIAN_POINT('Ctrl Pts',(1.63730653475049,1.,-1.33239425103694));
#33162=CARTESIAN_POINT('Ctrl Pts',(1.63116079730887,-1.,-1.33106149345618));
#33163=CARTESIAN_POINT('Ctrl Pts',(1.63116079730887,1.,-1.33106149345618));
#33164=CARTESIAN_POINT('Ctrl Pts',(1.62503464209777,-1.,-1.32969019505665));
#33165=CARTESIAN_POINT('Ctrl Pts',(1.62503464209777,1.,-1.32969019505665));
#33166=CARTESIAN_POINT('Ctrl Pts',(1.61892832270723,-1.,-1.32828000610448));
#33167=CARTESIAN_POINT('Ctrl Pts',(1.61892832270723,1.,-1.32828000610448));
#33168=CARTESIAN_POINT('Ctrl Pts',(1.61284234015762,-1.,-1.32683074483365));
#33169=CARTESIAN_POINT('Ctrl Pts',(1.61284234015762,1.,-1.32683074483365));
#33170=CARTESIAN_POINT('Ctrl Pts',(1.6067775829097,-1.,-1.32534250785794));
#33171=CARTESIAN_POINT('Ctrl Pts',(1.6067775829097,1.,-1.32534250785794));
#33172=CARTESIAN_POINT('Ctrl Pts',(1.600735118587,-1.,-1.32381550858266));
#33173=CARTESIAN_POINT('Ctrl Pts',(1.600735118587,1.,-1.32381550858266));
#33174=CARTESIAN_POINT('Ctrl Pts',(1.59471591079408,-1.,-1.32224985747686));
#33175=CARTESIAN_POINT('Ctrl Pts',(1.59471591079408,1.,-1.32224985747686));
#33176=CARTESIAN_POINT('Ctrl Pts',(1.58872057258244,-1.,-1.32064537110891));
#33177=CARTESIAN_POINT('Ctrl Pts',(1.58872057258244,1.,-1.32064537110891));
#33178=CARTESIAN_POINT('Ctrl Pts',(1.58274907898829,-1.,-1.31900135021428));
#33179=CARTESIAN_POINT('Ctrl Pts',(1.58274907898829,1.,-1.31900135021428));
#33180=CARTESIAN_POINT('Ctrl Pts',(1.57680056505585,-1.,-1.31731642317183));
#33181=CARTESIAN_POINT('Ctrl Pts',(1.57680056505585,1.,-1.31731642317183));
#33182=CARTESIAN_POINT('Ctrl Pts',(1.57087397835721,-1.,-1.31558903860015));
#33183=CARTESIAN_POINT('Ctrl Pts',(1.57087397835721,1.,-1.31558903860015));
#33184=CARTESIAN_POINT('Ctrl Pts',(1.56496872402352,-1.,-1.31381795281002));
#33185=CARTESIAN_POINT('Ctrl Pts',(1.56496872402352,1.,-1.31381795281002));
#33186=CARTESIAN_POINT('Ctrl Pts',(1.55908521254822,-1.,-1.31200264341696));
#33187=CARTESIAN_POINT('Ctrl Pts',(1.55908521254822,1.,-1.31200264341696));
#33188=CARTESIAN_POINT('Ctrl Pts',(1.55322568759481,-1.,-1.31014393684221));
#33189=CARTESIAN_POINT('Ctrl Pts',(1.55322568759481,1.,-1.31014393684221));
#33190=CARTESIAN_POINT('Ctrl Pts',(1.54739413957183,-1.,-1.30824393907471));
#33191=CARTESIAN_POINT('Ctrl Pts',(1.54739413957183,1.,-1.30824393907471));
#33192=CARTESIAN_POINT('Ctrl Pts',(1.54159462645428,-1.,-1.30630475189553));
#33193=CARTESIAN_POINT('Ctrl Pts',(1.54159462645428,1.,-1.30630475189553));
#33194=CARTESIAN_POINT('Ctrl Pts',(1.53582981268976,-1.,-1.30432735639487));
#33195=CARTESIAN_POINT('Ctrl Pts',(1.53582981268976,1.,-1.30432735639487));
#33196=CARTESIAN_POINT('Ctrl Pts',(1.53009970283893,-1.,-1.3023106439557));
#33197=CARTESIAN_POINT('Ctrl Pts',(1.53009970283893,1.,-1.3023106439557));
#33198=CARTESIAN_POINT('Ctrl Pts',(1.5243995786107,-1.,-1.30024984366334));
#33199=CARTESIAN_POINT('Ctrl Pts',(1.5243995786107,1.,-1.30024984366334));
#33200=CARTESIAN_POINT('Ctrl Pts',(1.51872184912735,-1.,-1.29813791800757));
#33201=CARTESIAN_POINT('Ctrl Pts',(1.51872184912735,1.,-1.29813791800757));
#33202=CARTESIAN_POINT('Ctrl Pts',(1.51305994241412,-1.,-1.29596850710518));
#33203=CARTESIAN_POINT('Ctrl Pts',(1.51305994241412,1.,-1.29596850710518));
#33204=CARTESIAN_POINT('Ctrl Pts',(1.50741159078367,-1.,-1.29373841372843));
#33205=CARTESIAN_POINT('Ctrl Pts',(1.50741159078367,1.,-1.29373841372843));
#33206=CARTESIAN_POINT('Ctrl Pts',(1.50178230149764,-1.,-1.29145022885171));
#33207=CARTESIAN_POINT('Ctrl Pts',(1.50178230149764,1.,-1.29145022885171));
#33208=CARTESIAN_POINT('Ctrl Pts',(1.49618896881729,-1.,-1.28911506584232));
#33209=CARTESIAN_POINT('Ctrl Pts',(1.49618896881729,1.,-1.28911506584232));
#33210=CARTESIAN_POINT('Ctrl Pts',(1.4906522831275,-1.,-1.28674676116415));
#33211=CARTESIAN_POINT('Ctrl Pts',(1.4906522831275,1.,-1.28674676116415));
#33212=CARTESIAN_POINT('Ctrl Pts',(1.48518817118891,-1.,-1.28435533880184));
#33213=CARTESIAN_POINT('Ctrl Pts',(1.48518817118891,1.,-1.28435533880184));
#33214=CARTESIAN_POINT('Ctrl Pts',(1.47980070347102,-1.,-1.28194158939522));
#33215=CARTESIAN_POINT('Ctrl Pts',(1.47980070347102,1.,-1.28194158939522));
#33216=CARTESIAN_POINT('Ctrl Pts',(1.4744717526711,-1.,-1.27948918248524));
#33217=CARTESIAN_POINT('Ctrl Pts',(1.4744717526711,1.,-1.27948918248524));
#33218=CARTESIAN_POINT('Ctrl Pts',(1.46916035917197,-1.,-1.27696414831144));
#33219=CARTESIAN_POINT('Ctrl Pts',(1.46916035917197,1.,-1.27696414831144));
#33220=CARTESIAN_POINT('Ctrl Pts',(1.4638243133254,-1.,-1.27433119897877));
#33221=CARTESIAN_POINT('Ctrl Pts',(1.4638243133254,1.,-1.27433119897877));
#33222=CARTESIAN_POINT('Ctrl Pts',(1.45843906294725,-1.,-1.27156805265312));
#33223=CARTESIAN_POINT('Ctrl Pts',(1.45843906294725,1.,-1.27156805265312));
#33224=CARTESIAN_POINT('Ctrl Pts',(1.45301422764205,-1.,-1.26867786804854));
#33225=CARTESIAN_POINT('Ctrl Pts',(1.45301422764205,1.,-1.26867786804854));
#33226=CARTESIAN_POINT('Ctrl Pts',(1.44761985001544,-1.,-1.26570925118767));
#33227=CARTESIAN_POINT('Ctrl Pts',(1.44761985001544,1.,-1.26570925118767));
#33228=CARTESIAN_POINT('Ctrl Pts',(1.44236470511145,-1.,-1.26273903323723));
#33229=CARTESIAN_POINT('Ctrl Pts',(1.44236470511145,1.,-1.26273903323723));
#33230=CARTESIAN_POINT('Ctrl Pts',(1.43734919180719,-1.,-1.25983531011894));
#33231=CARTESIAN_POINT('Ctrl Pts',(1.43734919180719,1.,-1.25983531011894));
#33232=CARTESIAN_POINT('Ctrl Pts',(1.43262645609679,-1.,-1.25702687965744));
#33233=CARTESIAN_POINT('Ctrl Pts',(1.43262645609679,1.,-1.25702687965744));
#33234=CARTESIAN_POINT('Ctrl Pts',(1.42815938799555,-1.,-1.25426945222783));
#33235=CARTESIAN_POINT('Ctrl Pts',(1.42815938799555,1.,-1.25426945222783));
#33236=CARTESIAN_POINT('Ctrl Pts',(1.42378102115911,-1.,-1.25141455570299));
#33237=CARTESIAN_POINT('Ctrl Pts',(1.42378102115911,1.,-1.25141455570299));
#33238=CARTESIAN_POINT('Ctrl Pts',(1.41923722596421,-1.,-1.24824430986911));
#33239=CARTESIAN_POINT('Ctrl Pts',(1.41923722596421,1.,-1.24824430986911));
#33240=CARTESIAN_POINT('Ctrl Pts',(1.41422913175437,-1.,-1.24450600513278));
#33241=CARTESIAN_POINT('Ctrl Pts',(1.41422913175437,1.,-1.24450600513278));
#33242=CARTESIAN_POINT('Ctrl Pts',(1.40845295531151,-1.,-1.23994455029421));
#33243=CARTESIAN_POINT('Ctrl Pts',(1.40845295531151,1.,-1.23994455029421));
#33244=CARTESIAN_POINT('Ctrl Pts',(1.40164708205345,-1.,-1.23434087289768));
#33245=CARTESIAN_POINT('Ctrl Pts',(1.40164708205345,1.,-1.23434087289768));
#33246=CARTESIAN_POINT('Ctrl Pts',(1.39361389567257,-1.,-1.22752961898063));
#33247=CARTESIAN_POINT('Ctrl Pts',(1.39361389567257,1.,-1.22752961898063));
#33248=CARTESIAN_POINT('Ctrl Pts',(1.38420564525391,-1.,-1.21938737278853));
#33249=CARTESIAN_POINT('Ctrl Pts',(1.38420564525391,1.,-1.21938737278853));
#33250=CARTESIAN_POINT('Ctrl Pts',(1.37331915604962,-1.,-1.20982812923113));
#33251=CARTESIAN_POINT('Ctrl Pts',(1.37331915604962,1.,-1.20982812923113));
#33252=CARTESIAN_POINT('Ctrl Pts',(1.36088705040677,-1.,-1.1987959077656));
#33253=CARTESIAN_POINT('Ctrl Pts',(1.36088705040677,1.,-1.1987959077656));
#33254=CARTESIAN_POINT('Ctrl Pts',(1.34687053998157,-1.,-1.18625865664915));
#33255=CARTESIAN_POINT('Ctrl Pts',(1.34687053998157,1.,-1.18625865664915));
#33256=CARTESIAN_POINT('Ctrl Pts',(1.33437539344842,-1.,-1.17501305787994));
#33257=CARTESIAN_POINT('Ctrl Pts',(1.33437539344842,1.,-1.17501305787994));
#33258=CARTESIAN_POINT('Ctrl Pts',(1.32428080720544,-1.,-1.16589330092532));
#33259=CARTESIAN_POINT('Ctrl Pts',(1.32428080720544,1.,-1.16589330092532));
#33260=CARTESIAN_POINT('Ctrl Pts',(1.3172297721596,-1.,-1.15950888730433));
#33261=CARTESIAN_POINT('Ctrl Pts',(1.3172297721596,1.,-1.15950888730433));
#33262=CARTESIAN_POINT('Ctrl Pts',(1.31362392696032,-1.,-1.15624053661742));
#33263=CARTESIAN_POINT('Ctrl Pts',(1.31362392696032,1.,-1.15624053661742));
#33264=CARTESIAN_POINT('',(1.73811241238545,1.,-1.34869019493419));
#33265=CARTESIAN_POINT('Ctrl Pts',(1.73811241238545,1.,-1.34869019493419));
#33266=CARTESIAN_POINT('Ctrl Pts',(1.73682580585819,1.,-1.34854391898145));
#33267=CARTESIAN_POINT('Ctrl Pts',(1.73425417886254,1.,-1.34824783113158));
#33268=CARTESIAN_POINT('Ctrl Pts',(1.73040149654497,1.,-1.3477930915247));
#33269=CARTESIAN_POINT('Ctrl Pts',(1.72527410681298,1.,-1.34716554820013));
#33270=CARTESIAN_POINT('Ctrl Pts',(1.7188807715095,1.,-1.34634568653586));
#33271=CARTESIAN_POINT('Ctrl Pts',(1.71250340687011,1.,-1.34549029589563));
#33272=CARTESIAN_POINT('Ctrl Pts',(1.70614212266676,1.,-1.34459924533783));
#33273=CARTESIAN_POINT('Ctrl Pts',(1.69979707754221,1.,-1.34367237124322));
#33274=CARTESIAN_POINT('Ctrl Pts',(1.6934684849664,1.,-1.34270948206139));
#33275=CARTESIAN_POINT('Ctrl Pts',(1.68715660868602,1.,-1.34171037484673));
#33276=CARTESIAN_POINT('Ctrl Pts',(1.68086176030308,1.,-1.3406748518516));
#33277=CARTESIAN_POINT('Ctrl Pts',(1.67458429426126,1.,-1.33960273470372));
#33278=CARTESIAN_POINT('Ctrl Pts',(1.66832460784078,1.,-1.33849388654458));
#33279=CARTESIAN_POINT('Ctrl Pts',(1.66208312542073,1.,-1.33734820885331));
#33280=CARTESIAN_POINT('Ctrl Pts',(1.65586025952651,1.,-1.33616559745217));
#33281=CARTESIAN_POINT('Ctrl Pts',(1.64965637286843,1.,-1.33494590468003));
#33282=CARTESIAN_POINT('Ctrl Pts',(1.64347174856007,1.,-1.33368890676554));
#33283=CARTESIAN_POINT('Ctrl Pts',(1.63730653475049,1.,-1.33239425103694));
#33284=CARTESIAN_POINT('Ctrl Pts',(1.63116079730887,1.,-1.33106149345618));
#33285=CARTESIAN_POINT('Ctrl Pts',(1.62503464209777,1.,-1.32969019505665));
#33286=CARTESIAN_POINT('Ctrl Pts',(1.61892832270723,1.,-1.32828000610448));
#33287=CARTESIAN_POINT('Ctrl Pts',(1.61284234015762,1.,-1.32683074483365));
#33288=CARTESIAN_POINT('Ctrl Pts',(1.6067775829097,1.,-1.32534250785794));
#33289=CARTESIAN_POINT('Ctrl Pts',(1.600735118587,1.,-1.32381550858266));
#33290=CARTESIAN_POINT('Ctrl Pts',(1.59471591079408,1.,-1.32224985747686));
#33291=CARTESIAN_POINT('Ctrl Pts',(1.58872057258244,1.,-1.32064537110891));
#33292=CARTESIAN_POINT('Ctrl Pts',(1.58274907898829,1.,-1.31900135021428));
#33293=CARTESIAN_POINT('Ctrl Pts',(1.57680056505585,1.,-1.31731642317183));
#33294=CARTESIAN_POINT('Ctrl Pts',(1.57087397835721,1.,-1.31558903860015));
#33295=CARTESIAN_POINT('Ctrl Pts',(1.56496872402352,1.,-1.31381795281002));
#33296=CARTESIAN_POINT('Ctrl Pts',(1.55908521254822,1.,-1.31200264341696));
#33297=CARTESIAN_POINT('Ctrl Pts',(1.55322568759481,1.,-1.31014393684221));
#33298=CARTESIAN_POINT('Ctrl Pts',(1.54739413957183,1.,-1.30824393907471));
#33299=CARTESIAN_POINT('Ctrl Pts',(1.54159462645428,1.,-1.30630475189553));
#33300=CARTESIAN_POINT('Ctrl Pts',(1.53582981268976,1.,-1.30432735639487));
#33301=CARTESIAN_POINT('Ctrl Pts',(1.53009970283893,1.,-1.3023106439557));
#33302=CARTESIAN_POINT('Ctrl Pts',(1.5243995786107,1.,-1.30024984366334));
#33303=CARTESIAN_POINT('Ctrl Pts',(1.51872184912735,1.,-1.29813791800757));
#33304=CARTESIAN_POINT('Ctrl Pts',(1.51305994241412,1.,-1.29596850710518));
#33305=CARTESIAN_POINT('Ctrl Pts',(1.50741159078367,1.,-1.29373841372843));
#33306=CARTESIAN_POINT('Ctrl Pts',(1.50178230149764,1.,-1.29145022885171));
#33307=CARTESIAN_POINT('Ctrl Pts',(1.49618896881729,1.,-1.28911506584232));
#33308=CARTESIAN_POINT('Ctrl Pts',(1.4906522831275,1.,-1.28674676116415));
#33309=CARTESIAN_POINT('Ctrl Pts',(1.48518817118891,1.,-1.28435533880184));
#33310=CARTESIAN_POINT('Ctrl Pts',(1.47980070347102,1.,-1.28194158939522));
#33311=CARTESIAN_POINT('Ctrl Pts',(1.4744717526711,1.,-1.27948918248524));
#33312=CARTESIAN_POINT('Ctrl Pts',(1.46916035917197,1.,-1.27696414831144));
#33313=CARTESIAN_POINT('Ctrl Pts',(1.4638243133254,1.,-1.27433119897877));
#33314=CARTESIAN_POINT('Ctrl Pts',(1.45843906294725,1.,-1.27156805265312));
#33315=CARTESIAN_POINT('Ctrl Pts',(1.45301422764205,1.,-1.26867786804854));
#33316=CARTESIAN_POINT('Ctrl Pts',(1.44761985001544,1.,-1.26570925118767));
#33317=CARTESIAN_POINT('Ctrl Pts',(1.44236470511145,1.,-1.26273903323723));
#33318=CARTESIAN_POINT('Ctrl Pts',(1.43734919180719,1.,-1.25983531011894));
#33319=CARTESIAN_POINT('Ctrl Pts',(1.43262645609679,1.,-1.25702687965744));
#33320=CARTESIAN_POINT('Ctrl Pts',(1.42815938799555,1.,-1.25426945222783));
#33321=CARTESIAN_POINT('Ctrl Pts',(1.42378102115911,1.,-1.25141455570299));
#33322=CARTESIAN_POINT('Ctrl Pts',(1.41923722596421,1.,-1.24824430986911));
#33323=CARTESIAN_POINT('Ctrl Pts',(1.41422913175437,1.,-1.24450600513278));
#33324=CARTESIAN_POINT('Ctrl Pts',(1.40845295531151,1.,-1.23994455029421));
#33325=CARTESIAN_POINT('Ctrl Pts',(1.40164708205345,1.,-1.23434087289768));
#33326=CARTESIAN_POINT('Ctrl Pts',(1.39361389567257,1.,-1.22752961898063));
#33327=CARTESIAN_POINT('Ctrl Pts',(1.38420564525391,1.,-1.21938737278853));
#33328=CARTESIAN_POINT('Ctrl Pts',(1.37331915604962,1.,-1.20982812923113));
#33329=CARTESIAN_POINT('Ctrl Pts',(1.36088705040677,1.,-1.1987959077656));
#33330=CARTESIAN_POINT('Ctrl Pts',(1.34687053998157,1.,-1.18625865664915));
#33331=CARTESIAN_POINT('Ctrl Pts',(1.33437539344842,1.,-1.17501305787994));
#33332=CARTESIAN_POINT('Ctrl Pts',(1.32428080720544,1.,-1.16589330092532));
#33333=CARTESIAN_POINT('Ctrl Pts',(1.3172297721596,1.,-1.15950888730433));
#33334=CARTESIAN_POINT('Ctrl Pts',(1.31362392696032,1.,-1.15624053661742));
#33335=CARTESIAN_POINT('',(1.73811241238545,0.,-1.34869019493419));
#33336=CARTESIAN_POINT('Origin',(1.81978687191668,0.,-1.23627494547115));
#33337=CARTESIAN_POINT('',(1.81978687191668,1.,-1.23627494547115));
#33338=CARTESIAN_POINT('',(1.73811241238545,1.,-1.34869019493419));
#33339=CARTESIAN_POINT('',(1.81978687191668,0.,-1.23627494547115));
#33340=CARTESIAN_POINT('Ctrl Pts',(1.5055822144029,-1.,-0.892032620296855));
#33341=CARTESIAN_POINT('Ctrl Pts',(1.5055822144029,1.,-0.892032620296855));
#33342=CARTESIAN_POINT('Ctrl Pts',(1.50980486807181,-1.,-0.894452006967538));
#33343=CARTESIAN_POINT('Ctrl Pts',(1.50980486807181,1.,-0.894452006967538));
#33344=CARTESIAN_POINT('Ctrl Pts',(1.51805569591479,-1.,-0.89918504749193));
#33345=CARTESIAN_POINT('Ctrl Pts',(1.51805569591479,1.,-0.89918504749193));
#33346=CARTESIAN_POINT('Ctrl Pts',(1.52984849890434,-1.,-0.905967409640499));
#33347=CARTESIAN_POINT('Ctrl Pts',(1.52984849890434,1.,-0.905967409640499));
#33348=CARTESIAN_POINT('Ctrl Pts',(1.54440491152807,-1.,-0.91437591904658));
#33349=CARTESIAN_POINT('Ctrl Pts',(1.54440491152807,1.,-0.91437591904658));
#33350=CARTESIAN_POINT('Ctrl Pts',(1.56065988582509,-1.,-0.923832188966322));
#33351=CARTESIAN_POINT('Ctrl Pts',(1.56065988582509,1.,-0.923832188966322));
#33352=CARTESIAN_POINT('Ctrl Pts',(1.57499388385561,-1.,-0.932246680128849));
#33353=CARTESIAN_POINT('Ctrl Pts',(1.57499388385561,1.,-0.932246680128849));
#33354=CARTESIAN_POINT('Ctrl Pts',(1.58744937489796,-1.,-0.939646377909319));
#33355=CARTESIAN_POINT('Ctrl Pts',(1.58744937489796,1.,-0.939646377909319));
#33356=CARTESIAN_POINT('Ctrl Pts',(1.59810042045408,-1.,-0.946078063325796));
#33357=CARTESIAN_POINT('Ctrl Pts',(1.59810042045408,1.,-0.946078063325796));
#33358=CARTESIAN_POINT('Ctrl Pts',(1.60706069897794,-1.,-0.951613284361248));
#33359=CARTESIAN_POINT('Ctrl Pts',(1.60706069897794,1.,-0.951613284361248));
#33360=CARTESIAN_POINT('Ctrl Pts',(1.61449324337233,-1.,-0.956354422921573));
#33361=CARTESIAN_POINT('Ctrl Pts',(1.61449324337233,1.,-0.956354422921573));
#33362=CARTESIAN_POINT('Ctrl Pts',(1.62061638139929,-1.,-0.960438326099958));
#33363=CARTESIAN_POINT('Ctrl Pts',(1.62061638139929,1.,-0.960438326099958));
#33364=CARTESIAN_POINT('Ctrl Pts',(1.6257193066974,-1.,-0.964046107037821));
#33365=CARTESIAN_POINT('Ctrl Pts',(1.6257193066974,1.,-0.964046107037821));
#33366=CARTESIAN_POINT('Ctrl Pts',(1.63013849959083,-1.,-0.967387853228041));
#33367=CARTESIAN_POINT('Ctrl Pts',(1.63013849959083,1.,-0.967387853228041));
#33368=CARTESIAN_POINT('Ctrl Pts',(1.63420665729609,-1.,-0.970669715996356));
#33369=CARTESIAN_POINT('Ctrl Pts',(1.63420665729609,1.,-0.970669715996356));
#33370=CARTESIAN_POINT('Ctrl Pts',(1.63820952658157,-1.,-0.974066058287501));
#33371=CARTESIAN_POINT('Ctrl Pts',(1.63820952658157,1.,-0.974066058287501));
#33372=CARTESIAN_POINT('Ctrl Pts',(1.64233990826831,-1.,-0.977689794120297));
#33373=CARTESIAN_POINT('Ctrl Pts',(1.64233990826831,1.,-0.977689794120297));
#33374=CARTESIAN_POINT('Ctrl Pts',(1.64665139190834,-1.,-0.981562530940574));
#33375=CARTESIAN_POINT('Ctrl Pts',(1.64665139190834,1.,-0.981562530940574));
#33376=CARTESIAN_POINT('Ctrl Pts',(1.6511001661277,-1.,-0.985642622921626));
#33377=CARTESIAN_POINT('Ctrl Pts',(1.6511001661277,1.,-0.985642622921626));
#33378=CARTESIAN_POINT('Ctrl Pts',(1.65559044289746,-1.,-0.98985562785445));
#33379=CARTESIAN_POINT('Ctrl Pts',(1.65559044289746,1.,-0.98985562785445));
#33380=CARTESIAN_POINT('Ctrl Pts',(1.66001553809916,-1.,-0.994121836661116));
#33381=CARTESIAN_POINT('Ctrl Pts',(1.66001553809916,1.,-0.994121836661116));
#33382=CARTESIAN_POINT('Ctrl Pts',(1.66430758030304,-1.,-0.998389654952317));
#33383=CARTESIAN_POINT('Ctrl Pts',(1.66430758030304,1.,-0.998389654952317));
#33384=CARTESIAN_POINT('Ctrl Pts',(1.66846059277231,-1.,-1.00265091003682));
#33385=CARTESIAN_POINT('Ctrl Pts',(1.66846059277231,1.,-1.00265091003682));
#33386=CARTESIAN_POINT('Ctrl Pts',(1.67250335383248,-1.,-1.00692206696387));
#33387=CARTESIAN_POINT('Ctrl Pts',(1.67250335383248,1.,-1.00692206696387));
#33388=CARTESIAN_POINT('Ctrl Pts',(1.67648246776457,-1.,-1.01123236493507));
#33389=CARTESIAN_POINT('Ctrl Pts',(1.67648246776457,1.,-1.01123236493507));
#33390=CARTESIAN_POINT('Ctrl Pts',(1.6804428989482,-1.,-1.01561026162787));
#33391=CARTESIAN_POINT('Ctrl Pts',(1.6804428989482,1.,-1.01561026162787));
#33392=CARTESIAN_POINT('Ctrl Pts',(1.68440578021739,-1.,-1.02006795074222));
#33393=CARTESIAN_POINT('Ctrl Pts',(1.68440578021739,1.,-1.02006795074222));
#33394=CARTESIAN_POINT('Ctrl Pts',(1.68836910178475,-1.,-1.02460180535272));
#33395=CARTESIAN_POINT('Ctrl Pts',(1.68836910178475,1.,-1.02460180535272));
#33396=CARTESIAN_POINT('Ctrl Pts',(1.69231840863471,-1.,-1.02919977579155));
#33397=CARTESIAN_POINT('Ctrl Pts',(1.69231840863471,1.,-1.02919977579155));
#33398=CARTESIAN_POINT('Ctrl Pts',(1.69623414782769,-1.,-1.03384646003587));
#33399=CARTESIAN_POINT('Ctrl Pts',(1.69623414782769,1.,-1.03384646003587));
#33400=CARTESIAN_POINT('Ctrl Pts',(1.70010052930951,-1.,-1.03852922490782));
#33401=CARTESIAN_POINT('Ctrl Pts',(1.70010052930951,1.,-1.03852922490782));
#33402=CARTESIAN_POINT('Ctrl Pts',(1.70391338707969,-1.,-1.04324363334546));
#33403=CARTESIAN_POINT('Ctrl Pts',(1.70391338707969,1.,-1.04324363334546));
#33404=CARTESIAN_POINT('Ctrl Pts',(1.70767646263641,-1.,-1.0479908540499));
#33405=CARTESIAN_POINT('Ctrl Pts',(1.70767646263641,1.,-1.0479908540499));
#33406=CARTESIAN_POINT('Ctrl Pts',(1.71139783543986,-1.,-1.05277517202854));
#33407=CARTESIAN_POINT('Ctrl Pts',(1.71139783543986,1.,-1.05277517202854));
#33408=CARTESIAN_POINT('Ctrl Pts',(1.71508654427022,-1.,-1.05760163192481));
#33409=CARTESIAN_POINT('Ctrl Pts',(1.71508654427022,1.,-1.05760163192481));
#33410=CARTESIAN_POINT('Ctrl Pts',(1.71874858456908,-1.,-1.0624732468065));
#33411=CARTESIAN_POINT('Ctrl Pts',(1.71874858456908,1.,-1.0624732468065));
#33412=CARTESIAN_POINT('Ctrl Pts',(1.72238500928456,-1.,-1.06738966975463));
#33413=CARTESIAN_POINT('Ctrl Pts',(1.72238500928456,1.,-1.06738966975463));
#33414=CARTESIAN_POINT('Ctrl Pts',(1.72599406198489,-1.,-1.07234866990252));
#33415=CARTESIAN_POINT('Ctrl Pts',(1.72599406198489,1.,-1.07234866990252));
#33416=CARTESIAN_POINT('Ctrl Pts',(1.72957248977424,-1.,-1.0773470373727));
#33417=CARTESIAN_POINT('Ctrl Pts',(1.72957248977424,1.,-1.0773470373727));
#33418=CARTESIAN_POINT('Ctrl Pts',(1.73311705663407,-1.,-1.08238162784749));
#33419=CARTESIAN_POINT('Ctrl Pts',(1.73311705663407,1.,-1.08238162784749));
#33420=CARTESIAN_POINT('Ctrl Pts',(1.73662628326093,-1.,-1.08745056285429));
#33421=CARTESIAN_POINT('Ctrl Pts',(1.73662628326093,1.,-1.08745056285429));
#33422=CARTESIAN_POINT('Ctrl Pts',(1.74010053962252,-1.,-1.09255329056496));
#33423=CARTESIAN_POINT('Ctrl Pts',(1.74010053962252,1.,-1.09255329056496));
#33424=CARTESIAN_POINT('Ctrl Pts',(1.74354119236212,-1.,-1.09768999241229));
#33425=CARTESIAN_POINT('Ctrl Pts',(1.74354119236212,1.,-1.09768999241229));
#33426=CARTESIAN_POINT('Ctrl Pts',(1.74695004214924,-1.,-1.10286118991144));
#33427=CARTESIAN_POINT('Ctrl Pts',(1.74695004214924,1.,-1.10286118991144));
#33428=CARTESIAN_POINT('Ctrl Pts',(1.75032866075914,-1.,-1.10806728183003));
#33429=CARTESIAN_POINT('Ctrl Pts',(1.75032866075914,1.,-1.10806728183003));
#33430=CARTESIAN_POINT('Ctrl Pts',(1.75367772094617,-1.,-1.11330807582542));
#33431=CARTESIAN_POINT('Ctrl Pts',(1.75367772094617,1.,-1.11330807582542));
#33432=CARTESIAN_POINT('Ctrl Pts',(1.75699720772089,-1.,-1.11858293216752));
#33433=CARTESIAN_POINT('Ctrl Pts',(1.75699720772089,1.,-1.11858293216752));
#33434=CARTESIAN_POINT('Ctrl Pts',(1.76028671825084,-1.,-1.12389096855078));
#33435=CARTESIAN_POINT('Ctrl Pts',(1.76028671825084,1.,-1.12389096855078));
#33436=CARTESIAN_POINT('Ctrl Pts',(1.76354571966171,-1.,-1.12923123555076));
#33437=CARTESIAN_POINT('Ctrl Pts',(1.76354571966171,1.,-1.12923123555076));
#33438=CARTESIAN_POINT('Ctrl Pts',(1.76677384551883,-1.,-1.13460291804635));
#33439=CARTESIAN_POINT('Ctrl Pts',(1.76677384551883,1.,-1.13460291804635));
#33440=CARTESIAN_POINT('Ctrl Pts',(1.76997111386806,-1.,-1.14000548337));
#33441=CARTESIAN_POINT('Ctrl Pts',(1.76997111386806,1.,-1.14000548337));
#33442=CARTESIAN_POINT('Ctrl Pts',(1.77313777896234,-1.,-1.14543858226948));
#33443=CARTESIAN_POINT('Ctrl Pts',(1.77313777896234,1.,-1.14543858226948));
#33444=CARTESIAN_POINT('Ctrl Pts',(1.77627422557034,-1.,-1.15090197841531));
#33445=CARTESIAN_POINT('Ctrl Pts',(1.77627422557034,1.,-1.15090197841531));
#33446=CARTESIAN_POINT('Ctrl Pts',(1.77938085564261,-1.,-1.15639547194689));
#33447=CARTESIAN_POINT('Ctrl Pts',(1.77938085564261,1.,-1.15639547194689));
#33448=CARTESIAN_POINT('Ctrl Pts',(1.78245795880949,-1.,-1.16191881298458));
#33449=CARTESIAN_POINT('Ctrl Pts',(1.78245795880949,1.,-1.16191881298458));
#33450=CARTESIAN_POINT('Ctrl Pts',(1.78550566040349,-1.,-1.16747166312239));
#33451=CARTESIAN_POINT('Ctrl Pts',(1.78550566040349,1.,-1.16747166312239));
#33452=CARTESIAN_POINT('Ctrl Pts',(1.78852398877523,-1.,-1.17305363177265));
#33453=CARTESIAN_POINT('Ctrl Pts',(1.78852398877523,1.,-1.17305363177265));
#33454=CARTESIAN_POINT('Ctrl Pts',(1.79151291552646,-1.,-1.17866429440781));
#33455=CARTESIAN_POINT('Ctrl Pts',(1.79151291552646,1.,-1.17866429440781));
#33456=CARTESIAN_POINT('Ctrl Pts',(1.79447240321572,-1.,-1.18430321697471));
#33457=CARTESIAN_POINT('Ctrl Pts',(1.79447240321572,1.,-1.18430321697471));
#33458=CARTESIAN_POINT('Ctrl Pts',(1.79740245923649,-1.,-1.1899699793456));
#33459=CARTESIAN_POINT('Ctrl Pts',(1.79740245923649,1.,-1.1899699793456));
#33460=CARTESIAN_POINT('Ctrl Pts',(1.80030314370121,-1.,-1.19566418930405));
#33461=CARTESIAN_POINT('Ctrl Pts',(1.80030314370121,1.,-1.19566418930405));
#33462=CARTESIAN_POINT('Ctrl Pts',(1.8031745483882,-1.,-1.2013854893912));
#33463=CARTESIAN_POINT('Ctrl Pts',(1.8031745483882,1.,-1.2013854893912));
#33464=CARTESIAN_POINT('Ctrl Pts',(1.80601678480772,-1.,-1.20713356605519));
#33465=CARTESIAN_POINT('Ctrl Pts',(1.80601678480772,1.,-1.20713356605519));
#33466=CARTESIAN_POINT('Ctrl Pts',(1.80882996916931,-1.,-1.2129081570818));
#33467=CARTESIAN_POINT('Ctrl Pts',(1.80882996916931,1.,-1.2129081570818));
#33468=CARTESIAN_POINT('Ctrl Pts',(1.81161420806172,-1.,-1.2187090610323));
#33469=CARTESIAN_POINT('Ctrl Pts',(1.81161420806172,1.,-1.2187090610323));
#33470=CARTESIAN_POINT('Ctrl Pts',(1.81436959209778,-1.,-1.22453613304507));
#33471=CARTESIAN_POINT('Ctrl Pts',(1.81436959209778,1.,-1.22453613304507));
#33472=CARTESIAN_POINT('Ctrl Pts',(1.81655087183054,-1.,-1.22921864890975));
#33473=CARTESIAN_POINT('Ctrl Pts',(1.81655087183054,1.,-1.22921864890975));
#33474=CARTESIAN_POINT('Ctrl Pts',(1.81817389920914,-1.,-1.23274224526804));
#33475=CARTESIAN_POINT('Ctrl Pts',(1.81817389920914,1.,-1.23274224526804));
#33476=CARTESIAN_POINT('Ctrl Pts',(1.81925017193531,-1.,-1.23509651170384));
#33477=CARTESIAN_POINT('Ctrl Pts',(1.81925017193531,1.,-1.23509651170384));
#33478=CARTESIAN_POINT('Ctrl Pts',(1.81978687191668,-1.,-1.23627494547115));
#33479=CARTESIAN_POINT('Ctrl Pts',(1.81978687191668,1.,-1.23627494547115));
#33480=CARTESIAN_POINT('',(1.5055822144029,1.,-0.892032620296855));
#33481=CARTESIAN_POINT('Ctrl Pts',(1.5055822144029,1.,-0.892032620296855));
#33482=CARTESIAN_POINT('Ctrl Pts',(1.50980486807181,1.,-0.894452006967538));
#33483=CARTESIAN_POINT('Ctrl Pts',(1.51805569591479,1.,-0.89918504749193));
#33484=CARTESIAN_POINT('Ctrl Pts',(1.52984849890434,1.,-0.905967409640499));
#33485=CARTESIAN_POINT('Ctrl Pts',(1.54440491152807,1.,-0.91437591904658));
#33486=CARTESIAN_POINT('Ctrl Pts',(1.56065988582509,1.,-0.923832188966322));
#33487=CARTESIAN_POINT('Ctrl Pts',(1.57499388385561,1.,-0.932246680128849));
#33488=CARTESIAN_POINT('Ctrl Pts',(1.58744937489796,1.,-0.939646377909319));
#33489=CARTESIAN_POINT('Ctrl Pts',(1.59810042045408,1.,-0.946078063325796));
#33490=CARTESIAN_POINT('Ctrl Pts',(1.60706069897794,1.,-0.951613284361248));
#33491=CARTESIAN_POINT('Ctrl Pts',(1.61449324337233,1.,-0.956354422921573));
#33492=CARTESIAN_POINT('Ctrl Pts',(1.62061638139929,1.,-0.960438326099958));
#33493=CARTESIAN_POINT('Ctrl Pts',(1.6257193066974,1.,-0.964046107037821));
#33494=CARTESIAN_POINT('Ctrl Pts',(1.63013849959083,1.,-0.967387853228041));
#33495=CARTESIAN_POINT('Ctrl Pts',(1.63420665729609,1.,-0.970669715996356));
#33496=CARTESIAN_POINT('Ctrl Pts',(1.63820952658157,1.,-0.974066058287501));
#33497=CARTESIAN_POINT('Ctrl Pts',(1.64233990826831,1.,-0.977689794120297));
#33498=CARTESIAN_POINT('Ctrl Pts',(1.64665139190834,1.,-0.981562530940574));
#33499=CARTESIAN_POINT('Ctrl Pts',(1.6511001661277,1.,-0.985642622921626));
#33500=CARTESIAN_POINT('Ctrl Pts',(1.65559044289746,1.,-0.98985562785445));
#33501=CARTESIAN_POINT('Ctrl Pts',(1.66001553809916,1.,-0.994121836661116));
#33502=CARTESIAN_POINT('Ctrl Pts',(1.66430758030304,1.,-0.998389654952317));
#33503=CARTESIAN_POINT('Ctrl Pts',(1.66846059277231,1.,-1.00265091003682));
#33504=CARTESIAN_POINT('Ctrl Pts',(1.67250335383248,1.,-1.00692206696387));
#33505=CARTESIAN_POINT('Ctrl Pts',(1.67648246776457,1.,-1.01123236493507));
#33506=CARTESIAN_POINT('Ctrl Pts',(1.6804428989482,1.,-1.01561026162787));
#33507=CARTESIAN_POINT('Ctrl Pts',(1.68440578021739,1.,-1.02006795074222));
#33508=CARTESIAN_POINT('Ctrl Pts',(1.68836910178475,1.,-1.02460180535272));
#33509=CARTESIAN_POINT('Ctrl Pts',(1.69231840863471,1.,-1.02919977579155));
#33510=CARTESIAN_POINT('Ctrl Pts',(1.69623414782769,1.,-1.03384646003587));
#33511=CARTESIAN_POINT('Ctrl Pts',(1.70010052930951,1.,-1.03852922490782));
#33512=CARTESIAN_POINT('Ctrl Pts',(1.70391338707969,1.,-1.04324363334546));
#33513=CARTESIAN_POINT('Ctrl Pts',(1.70767646263641,1.,-1.0479908540499));
#33514=CARTESIAN_POINT('Ctrl Pts',(1.71139783543986,1.,-1.05277517202854));
#33515=CARTESIAN_POINT('Ctrl Pts',(1.71508654427022,1.,-1.05760163192481));
#33516=CARTESIAN_POINT('Ctrl Pts',(1.71874858456908,1.,-1.0624732468065));
#33517=CARTESIAN_POINT('Ctrl Pts',(1.72238500928456,1.,-1.06738966975463));
#33518=CARTESIAN_POINT('Ctrl Pts',(1.72599406198489,1.,-1.07234866990252));
#33519=CARTESIAN_POINT('Ctrl Pts',(1.72957248977424,1.,-1.0773470373727));
#33520=CARTESIAN_POINT('Ctrl Pts',(1.73311705663407,1.,-1.08238162784749));
#33521=CARTESIAN_POINT('Ctrl Pts',(1.73662628326093,1.,-1.08745056285429));
#33522=CARTESIAN_POINT('Ctrl Pts',(1.74010053962252,1.,-1.09255329056496));
#33523=CARTESIAN_POINT('Ctrl Pts',(1.74354119236212,1.,-1.09768999241229));
#33524=CARTESIAN_POINT('Ctrl Pts',(1.74695004214924,1.,-1.10286118991144));
#33525=CARTESIAN_POINT('Ctrl Pts',(1.75032866075914,1.,-1.10806728183003));
#33526=CARTESIAN_POINT('Ctrl Pts',(1.75367772094617,1.,-1.11330807582542));
#33527=CARTESIAN_POINT('Ctrl Pts',(1.75699720772089,1.,-1.11858293216752));
#33528=CARTESIAN_POINT('Ctrl Pts',(1.76028671825084,1.,-1.12389096855078));
#33529=CARTESIAN_POINT('Ctrl Pts',(1.76354571966171,1.,-1.12923123555076));
#33530=CARTESIAN_POINT('Ctrl Pts',(1.76677384551883,1.,-1.13460291804635));
#33531=CARTESIAN_POINT('Ctrl Pts',(1.76997111386806,1.,-1.14000548337));
#33532=CARTESIAN_POINT('Ctrl Pts',(1.77313777896234,1.,-1.14543858226948));
#33533=CARTESIAN_POINT('Ctrl Pts',(1.77627422557034,1.,-1.15090197841531));
#33534=CARTESIAN_POINT('Ctrl Pts',(1.77938085564261,1.,-1.15639547194689));
#33535=CARTESIAN_POINT('Ctrl Pts',(1.78245795880949,1.,-1.16191881298458));
#33536=CARTESIAN_POINT('Ctrl Pts',(1.78550566040349,1.,-1.16747166312239));
#33537=CARTESIAN_POINT('Ctrl Pts',(1.78852398877523,1.,-1.17305363177265));
#33538=CARTESIAN_POINT('Ctrl Pts',(1.79151291552646,1.,-1.17866429440781));
#33539=CARTESIAN_POINT('Ctrl Pts',(1.79447240321572,1.,-1.18430321697471));
#33540=CARTESIAN_POINT('Ctrl Pts',(1.79740245923649,1.,-1.1899699793456));
#33541=CARTESIAN_POINT('Ctrl Pts',(1.80030314370121,1.,-1.19566418930405));
#33542=CARTESIAN_POINT('Ctrl Pts',(1.8031745483882,1.,-1.2013854893912));
#33543=CARTESIAN_POINT('Ctrl Pts',(1.80601678480772,1.,-1.20713356605519));
#33544=CARTESIAN_POINT('Ctrl Pts',(1.80882996916931,1.,-1.2129081570818));
#33545=CARTESIAN_POINT('Ctrl Pts',(1.81161420806172,1.,-1.2187090610323));
#33546=CARTESIAN_POINT('Ctrl Pts',(1.81436959209778,1.,-1.22453613304507));
#33547=CARTESIAN_POINT('Ctrl Pts',(1.81655087183054,1.,-1.22921864890975));
#33548=CARTESIAN_POINT('Ctrl Pts',(1.81817389920914,1.,-1.23274224526804));
#33549=CARTESIAN_POINT('Ctrl Pts',(1.81925017193531,1.,-1.23509651170384));
#33550=CARTESIAN_POINT('Ctrl Pts',(1.81978687191668,1.,-1.23627494547115));
#33551=CARTESIAN_POINT('',(1.5055822144029,0.,-0.892032620296855));
#33552=CARTESIAN_POINT('Origin',(0.,0.,0.));
#33553=CARTESIAN_POINT('',(1.60662857109684,1.,-0.693717979106306));
#33554=CARTESIAN_POINT('Origin',(0.,1.,0.));
#33555=CARTESIAN_POINT('',(1.60662857109684,0.,-0.693717979106308));
#33556=CARTESIAN_POINT('Ctrl Pts',(2.0698113262342,-1.,-0.745574324794401));
#33557=CARTESIAN_POINT('Ctrl Pts',(2.0698113262342,1.,-0.745574324794401));
#33558=CARTESIAN_POINT('Ctrl Pts',(2.06854248895728,-1.,-0.745832791378367));
#33559=CARTESIAN_POINT('Ctrl Pts',(2.06854248895728,1.,-0.745832791378367));
#33560=CARTESIAN_POINT('Ctrl Pts',(2.06600523016815,-1.,-0.746345871544201));
#33561=CARTESIAN_POINT('Ctrl Pts',(2.06600523016815,1.,-0.746345871544201));
#33562=CARTESIAN_POINT('Ctrl Pts',(2.06220058927826,-1.,-0.74710393278792));
#33563=CARTESIAN_POINT('Ctrl Pts',(2.06220058927826,1.,-0.74710393278792));
#33564=CARTESIAN_POINT('Ctrl Pts',(2.05713023031006,-1.,-0.748091554183803));
#33565=CARTESIAN_POINT('Ctrl Pts',(2.05713023031006,1.,-0.748091554183803));
#33566=CARTESIAN_POINT('Ctrl Pts',(2.05079645592154,-1.,-0.749287468665046));
#33567=CARTESIAN_POINT('Ctrl Pts',(2.05079645592154,1.,-0.749287468665046));
#33568=CARTESIAN_POINT('Ctrl Pts',(2.04446689147979,-1.,-0.750444657875576));
#33569=CARTESIAN_POINT('Ctrl Pts',(2.04446689147979,1.,-0.750444657875576));
#33570=CARTESIAN_POINT('Ctrl Pts',(2.03814160092099,-1.,-0.751562963361115));
#33571=CARTESIAN_POINT('Ctrl Pts',(2.03814160092099,1.,-0.751562963361115));
#33572=CARTESIAN_POINT('Ctrl Pts',(2.03182068456221,-1.,-0.752642180487211));
#33573=CARTESIAN_POINT('Ctrl Pts',(2.03182068456221,1.,-0.752642180487211));
#33574=CARTESIAN_POINT('Ctrl Pts',(2.02550428623313,-1.,-0.753682061112768));
#33575=CARTESIAN_POINT('Ctrl Pts',(2.02550428623313,1.,-0.753682061112768));
#33576=CARTESIAN_POINT('Ctrl Pts',(2.01919259405809,-1.,-0.754682330722816));
#33577=CARTESIAN_POINT('Ctrl Pts',(2.01919259405809,1.,-0.754682330722816));
#33578=CARTESIAN_POINT('Ctrl Pts',(2.01288584328084,-1.,-0.755642704957865));
#33579=CARTESIAN_POINT('Ctrl Pts',(2.01288584328084,1.,-0.755642704957865));
#33580=CARTESIAN_POINT('Ctrl Pts',(2.0065843158773,-1.,-0.756562904646671));
#33581=CARTESIAN_POINT('Ctrl Pts',(2.0065843158773,1.,-0.756562904646671));
#33582=CARTESIAN_POINT('Ctrl Pts',(2.00028834739178,-1.,-0.757442676862724));
#33583=CARTESIAN_POINT('Ctrl Pts',(2.00028834739178,1.,-0.757442676862724));
#33584=CARTESIAN_POINT('Ctrl Pts',(1.99399831098817,-1.,-0.758281796766761));
#33585=CARTESIAN_POINT('Ctrl Pts',(1.99399831098817,1.,-0.758281796766761));
#33586=CARTESIAN_POINT('Ctrl Pts',(1.98771456680874,-1.,-0.759080037802488));
#33587=CARTESIAN_POINT('Ctrl Pts',(1.98771456680874,1.,-0.759080037802488));
#33588=CARTESIAN_POINT('Ctrl Pts',(1.98143741418172,-1.,-0.75983714745219));
#33589=CARTESIAN_POINT('Ctrl Pts',(1.98143741418172,1.,-0.75983714745219));
#33590=CARTESIAN_POINT('Ctrl Pts',(1.97516705321494,-1.,-0.760552825409757));
#33591=CARTESIAN_POINT('Ctrl Pts',(1.97516705321494,1.,-0.760552825409757));
#33592=CARTESIAN_POINT('Ctrl Pts',(1.96890351582499,-1.,-0.761226690483821));
#33593=CARTESIAN_POINT('Ctrl Pts',(1.96890351582499,1.,-0.761226690483821));
#33594=CARTESIAN_POINT('Ctrl Pts',(1.96264672744186,-1.,-0.761858300014424));
#33595=CARTESIAN_POINT('Ctrl Pts',(1.96264672744186,1.,-0.761858300014424));
#33596=CARTESIAN_POINT('Ctrl Pts',(1.95639665309869,-1.,-0.762447203806179));
#33597=CARTESIAN_POINT('Ctrl Pts',(1.95639665309869,1.,-0.762447203806179));
#33598=CARTESIAN_POINT('Ctrl Pts',(1.95015342590024,-1.,-0.762992990878769));
#33599=CARTESIAN_POINT('Ctrl Pts',(1.95015342590024,1.,-0.762992990878769));
#33600=CARTESIAN_POINT('Ctrl Pts',(1.9439174661764,-1.,-0.763495333538629));
#33601=CARTESIAN_POINT('Ctrl Pts',(1.9439174661764,1.,-0.763495333538629));
#33602=CARTESIAN_POINT('Ctrl Pts',(1.93768964875886,-1.,-0.763954049121459));
#33603=CARTESIAN_POINT('Ctrl Pts',(1.93768964875886,1.,-0.763954049121459));
#33604=CARTESIAN_POINT('Ctrl Pts',(1.93147105496382,-1.,-0.764369010673941));
#33605=CARTESIAN_POINT('Ctrl Pts',(1.93147105496382,1.,-0.764369010673941));
#33606=CARTESIAN_POINT('Ctrl Pts',(1.92526263537048,-1.,-0.764740025488212));
#33607=CARTESIAN_POINT('Ctrl Pts',(1.92526263537048,1.,-0.764740025488212));
#33608=CARTESIAN_POINT('Ctrl Pts',(1.91906491634196,-1.,-0.765066729667089));
#33609=CARTESIAN_POINT('Ctrl Pts',(1.91906491634196,1.,-0.765066729667089));
#33610=CARTESIAN_POINT('Ctrl Pts',(1.91287765805169,-1.,-0.765348465884722));
#33611=CARTESIAN_POINT('Ctrl Pts',(1.91287765805169,1.,-0.765348465884722));
#33612=CARTESIAN_POINT('Ctrl Pts',(1.90669961402356,-1.,-0.765584196937919));
#33613=CARTESIAN_POINT('Ctrl Pts',(1.90669961402356,1.,-0.765584196937919));
#33614=CARTESIAN_POINT('Ctrl Pts',(1.90052930393596,-1.,-0.765772772593386));
#33615=CARTESIAN_POINT('Ctrl Pts',(1.90052930393596,1.,-0.765772772593386));
#33616=CARTESIAN_POINT('Ctrl Pts',(1.89436577771388,-1.,-0.765913193856978));
#33617=CARTESIAN_POINT('Ctrl Pts',(1.89436577771388,1.,-0.765913193856978));
#33618=CARTESIAN_POINT('Ctrl Pts',(1.88820926433409,-1.,-0.766004837062091));
#33619=CARTESIAN_POINT('Ctrl Pts',(1.88820926433409,1.,-0.766004837062091));
#33620=CARTESIAN_POINT('Ctrl Pts',(1.88206215302561,-1.,-0.766047794851865));
#33621=CARTESIAN_POINT('Ctrl Pts',(1.88206215302561,1.,-0.766047794851865));
#33622=CARTESIAN_POINT('Ctrl Pts',(1.87592888967883,-1.,-0.766042837036744));
#33623=CARTESIAN_POINT('Ctrl Pts',(1.87592888967883,1.,-0.766042837036744));
#33624=CARTESIAN_POINT('Ctrl Pts',(1.86981398314341,-1.,-0.765990708546091));
#33625=CARTESIAN_POINT('Ctrl Pts',(1.86981398314341,1.,-0.765990708546091));
#33626=CARTESIAN_POINT('Ctrl Pts',(1.86372027063312,-1.,-0.765891519092547));
#33627=CARTESIAN_POINT('Ctrl Pts',(1.86372027063312,1.,-0.765891519092547));
#33628=CARTESIAN_POINT('Ctrl Pts',(1.85764741390394,-1.,-0.765744212909319));
#33629=CARTESIAN_POINT('Ctrl Pts',(1.85764741390394,1.,-0.765744212909319));
#33630=CARTESIAN_POINT('Ctrl Pts',(1.85158945130063,-1.,-0.765545710619063));
#33631=CARTESIAN_POINT('Ctrl Pts',(1.85158945130063,1.,-0.765545710619063));
#33632=CARTESIAN_POINT('Ctrl Pts',(1.84553698875924,-1.,-0.765291664862029));
#33633=CARTESIAN_POINT('Ctrl Pts',(1.84553698875924,1.,-0.765291664862029));
#33634=CARTESIAN_POINT('Ctrl Pts',(1.83948181064835,-1.,-0.764978057881738));
#33635=CARTESIAN_POINT('Ctrl Pts',(1.83948181064835,1.,-0.764978057881738));
#33636=CARTESIAN_POINT('Ctrl Pts',(1.83342077227142,-1.,-0.764602549687853));
#33637=CARTESIAN_POINT('Ctrl Pts',(1.83342077227142,1.,-0.764602549687853));
#33638=CARTESIAN_POINT('Ctrl Pts',(1.82735991200065,-1.,-0.764165902605995));
#33639=CARTESIAN_POINT('Ctrl Pts',(1.82735991200065,1.,-0.764165902605995));
#33640=CARTESIAN_POINT('Ctrl Pts',(1.82131873145266,-1.,-0.763673465462727));
#33641=CARTESIAN_POINT('Ctrl Pts',(1.82131873145266,1.,-0.763673465462727));
#33642=CARTESIAN_POINT('Ctrl Pts',(1.8153211840553,-1.,-0.763132003836634));
#33643=CARTESIAN_POINT('Ctrl Pts',(1.8153211840553,1.,-0.763132003836634));
#33644=CARTESIAN_POINT('Ctrl Pts',(1.80938551463965,-1.,-0.762546129463938));
#33645=CARTESIAN_POINT('Ctrl Pts',(1.80938551463965,1.,-0.762546129463938));
#33646=CARTESIAN_POINT('Ctrl Pts',(1.80351583877342,-1.,-0.761915336443547));
#33647=CARTESIAN_POINT('Ctrl Pts',(1.80351583877342,1.,-0.761915336443547));
#33648=CARTESIAN_POINT('Ctrl Pts',(1.79768986997783,-1.,-0.761229695230558));
#33649=CARTESIAN_POINT('Ctrl Pts',(1.79768986997783,1.,-0.761229695230558));
#33650=CARTESIAN_POINT('Ctrl Pts',(1.7918581561088,-1.,-0.760469555880749));
#33651=CARTESIAN_POINT('Ctrl Pts',(1.7918581561088,1.,-0.760469555880749));
#33652=CARTESIAN_POINT('Ctrl Pts',(1.78596964884604,-1.,-0.75961440111019));
#33653=CARTESIAN_POINT('Ctrl Pts',(1.78596964884604,1.,-0.75961440111019));
#33654=CARTESIAN_POINT('Ctrl Pts',(1.77999411220945,-1.,-0.758650626677519));
#33655=CARTESIAN_POINT('Ctrl Pts',(1.77999411220945,1.,-0.758650626677519));
#33656=CARTESIAN_POINT('Ctrl Pts',(1.77394167108292,-1.,-0.757578264077029));
#33657=CARTESIAN_POINT('Ctrl Pts',(1.77394167108292,1.,-0.757578264077029));
#33658=CARTESIAN_POINT('Ctrl Pts',(1.76789396002998,-1.,-0.75642189602781));
#33659=CARTESIAN_POINT('Ctrl Pts',(1.76789396002998,1.,-0.75642189602781));
#33660=CARTESIAN_POINT('Ctrl Pts',(1.76197817240128,-1.,-0.755220979974462));
#33661=CARTESIAN_POINT('Ctrl Pts',(1.76197817240128,1.,-0.755220979974462));
#33662=CARTESIAN_POINT('Ctrl Pts',(1.75631083600019,-1.,-0.754009254027829));
#33663=CARTESIAN_POINT('Ctrl Pts',(1.75631083600019,1.,-0.754009254027829));
#33664=CARTESIAN_POINT('Ctrl Pts',(1.75095139468794,-1.,-0.752797683531314));
#33665=CARTESIAN_POINT('Ctrl Pts',(1.75095139468794,1.,-0.752797683531314));
#33666=CARTESIAN_POINT('Ctrl Pts',(1.74585086852502,-1.,-0.751555614164483));
#33667=CARTESIAN_POINT('Ctrl Pts',(1.74585086852502,1.,-0.751555614164483));
#33668=CARTESIAN_POINT('Ctrl Pts',(1.74080458267114,-1.,-0.75019343598125));
#33669=CARTESIAN_POINT('Ctrl Pts',(1.74080458267114,1.,-0.75019343598125));
#33670=CARTESIAN_POINT('Ctrl Pts',(1.7355035168033,-1.,-0.74858246295687));
#33671=CARTESIAN_POINT('Ctrl Pts',(1.7355035168033,1.,-0.74858246295687));
#33672=CARTESIAN_POINT('Ctrl Pts',(1.72958533647714,-1.,-0.746574710097752));
#33673=CARTESIAN_POINT('Ctrl Pts',(1.72958533647714,1.,-0.746574710097752));
#33674=CARTESIAN_POINT('Ctrl Pts',(1.72268229916769,-1.,-0.744021445433094));
#33675=CARTESIAN_POINT('Ctrl Pts',(1.72268229916769,1.,-0.744021445433094));
#33676=CARTESIAN_POINT('Ctrl Pts',(1.71447789751001,-1.,-0.74079516202821));
#33677=CARTESIAN_POINT('Ctrl Pts',(1.71447789751001,1.,-0.74079516202821));
#33678=CARTESIAN_POINT('Ctrl Pts',(1.70473309004249,-1.,-0.736799665716932));
#33679=CARTESIAN_POINT('Ctrl Pts',(1.70473309004249,1.,-0.736799665716932));
#33680=CARTESIAN_POINT('Ctrl Pts',(1.69326921972915,-1.,-0.731963238685357));
#33681=CARTESIAN_POINT('Ctrl Pts',(1.69326921972915,1.,-0.731963238685357));
#33682=CARTESIAN_POINT('Ctrl Pts',(1.67996158451922,-1.,-0.726235967982445));
#33683=CARTESIAN_POINT('Ctrl Pts',(1.67996158451922,1.,-0.726235967982445));
#33684=CARTESIAN_POINT('Ctrl Pts',(1.66472880551777,-1.,-0.71958543378795));
#33685=CARTESIAN_POINT('Ctrl Pts',(1.66472880551777,1.,-0.71958543378795));
#33686=CARTESIAN_POINT('Ctrl Pts',(1.64752408828442,-1.,-0.711993139340448));
#33687=CARTESIAN_POINT('Ctrl Pts',(1.64752408828442,1.,-0.711993139340448));
#33688=CARTESIAN_POINT('Ctrl Pts',(1.6321654166204,-1.,-0.705159151977294));
#33689=CARTESIAN_POINT('Ctrl Pts',(1.6321654166204,1.,-0.705159151977294));
#33690=CARTESIAN_POINT('Ctrl Pts',(1.61974673471117,-1.,-0.699605146398837));
#33691=CARTESIAN_POINT('Ctrl Pts',(1.61974673471117,1.,-0.699605146398837));
#33692=CARTESIAN_POINT('Ctrl Pts',(1.61106790957619,-1.,-0.69571209787897));
#33693=CARTESIAN_POINT('Ctrl Pts',(1.61106790957619,1.,-0.69571209787897));
#33694=CARTESIAN_POINT('Ctrl Pts',(1.60662857109684,-1.,-0.693717979106306));
#33695=CARTESIAN_POINT('Ctrl Pts',(1.60662857109684,1.,-0.693717979106306));
#33696=CARTESIAN_POINT('',(2.0698113262342,1.,-0.745574324794401));
#33697=CARTESIAN_POINT('Ctrl Pts',(2.0698113262342,1.,-0.745574324794401));
#33698=CARTESIAN_POINT('Ctrl Pts',(2.06854248895728,1.,-0.745832791378367));
#33699=CARTESIAN_POINT('Ctrl Pts',(2.06600523016815,1.,-0.746345871544201));
#33700=CARTESIAN_POINT('Ctrl Pts',(2.06220058927826,1.,-0.74710393278792));
#33701=CARTESIAN_POINT('Ctrl Pts',(2.05713023031006,1.,-0.748091554183803));
#33702=CARTESIAN_POINT('Ctrl Pts',(2.05079645592154,1.,-0.749287468665046));
#33703=CARTESIAN_POINT('Ctrl Pts',(2.04446689147979,1.,-0.750444657875576));
#33704=CARTESIAN_POINT('Ctrl Pts',(2.03814160092099,1.,-0.751562963361115));
#33705=CARTESIAN_POINT('Ctrl Pts',(2.03182068456221,1.,-0.752642180487211));
#33706=CARTESIAN_POINT('Ctrl Pts',(2.02550428623313,1.,-0.753682061112768));
#33707=CARTESIAN_POINT('Ctrl Pts',(2.01919259405809,1.,-0.754682330722816));
#33708=CARTESIAN_POINT('Ctrl Pts',(2.01288584328084,1.,-0.755642704957865));
#33709=CARTESIAN_POINT('Ctrl Pts',(2.0065843158773,1.,-0.756562904646671));
#33710=CARTESIAN_POINT('Ctrl Pts',(2.00028834739178,1.,-0.757442676862724));
#33711=CARTESIAN_POINT('Ctrl Pts',(1.99399831098817,1.,-0.758281796766761));
#33712=CARTESIAN_POINT('Ctrl Pts',(1.98771456680874,1.,-0.759080037802488));
#33713=CARTESIAN_POINT('Ctrl Pts',(1.98143741418172,1.,-0.75983714745219));
#33714=CARTESIAN_POINT('Ctrl Pts',(1.97516705321494,1.,-0.760552825409757));
#33715=CARTESIAN_POINT('Ctrl Pts',(1.96890351582499,1.,-0.761226690483821));
#33716=CARTESIAN_POINT('Ctrl Pts',(1.96264672744186,1.,-0.761858300014424));
#33717=CARTESIAN_POINT('Ctrl Pts',(1.95639665309869,1.,-0.762447203806179));
#33718=CARTESIAN_POINT('Ctrl Pts',(1.95015342590024,1.,-0.762992990878769));
#33719=CARTESIAN_POINT('Ctrl Pts',(1.9439174661764,1.,-0.763495333538629));
#33720=CARTESIAN_POINT('Ctrl Pts',(1.93768964875886,1.,-0.763954049121459));
#33721=CARTESIAN_POINT('Ctrl Pts',(1.93147105496382,1.,-0.764369010673941));
#33722=CARTESIAN_POINT('Ctrl Pts',(1.92526263537048,1.,-0.764740025488212));
#33723=CARTESIAN_POINT('Ctrl Pts',(1.91906491634196,1.,-0.765066729667089));
#33724=CARTESIAN_POINT('Ctrl Pts',(1.91287765805169,1.,-0.765348465884722));
#33725=CARTESIAN_POINT('Ctrl Pts',(1.90669961402356,1.,-0.765584196937919));
#33726=CARTESIAN_POINT('Ctrl Pts',(1.90052930393596,1.,-0.765772772593386));
#33727=CARTESIAN_POINT('Ctrl Pts',(1.89436577771388,1.,-0.765913193856978));
#33728=CARTESIAN_POINT('Ctrl Pts',(1.88820926433409,1.,-0.766004837062091));
#33729=CARTESIAN_POINT('Ctrl Pts',(1.88206215302561,1.,-0.766047794851865));
#33730=CARTESIAN_POINT('Ctrl Pts',(1.87592888967883,1.,-0.766042837036744));
#33731=CARTESIAN_POINT('Ctrl Pts',(1.86981398314341,1.,-0.765990708546091));
#33732=CARTESIAN_POINT('Ctrl Pts',(1.86372027063312,1.,-0.765891519092547));
#33733=CARTESIAN_POINT('Ctrl Pts',(1.85764741390394,1.,-0.765744212909319));
#33734=CARTESIAN_POINT('Ctrl Pts',(1.85158945130063,1.,-0.765545710619063));
#33735=CARTESIAN_POINT('Ctrl Pts',(1.84553698875924,1.,-0.765291664862029));
#33736=CARTESIAN_POINT('Ctrl Pts',(1.83948181064835,1.,-0.764978057881738));
#33737=CARTESIAN_POINT('Ctrl Pts',(1.83342077227142,1.,-0.764602549687853));
#33738=CARTESIAN_POINT('Ctrl Pts',(1.82735991200065,1.,-0.764165902605995));
#33739=CARTESIAN_POINT('Ctrl Pts',(1.82131873145266,1.,-0.763673465462727));
#33740=CARTESIAN_POINT('Ctrl Pts',(1.8153211840553,1.,-0.763132003836634));
#33741=CARTESIAN_POINT('Ctrl Pts',(1.80938551463965,1.,-0.762546129463938));
#33742=CARTESIAN_POINT('Ctrl Pts',(1.80351583877342,1.,-0.761915336443547));
#33743=CARTESIAN_POINT('Ctrl Pts',(1.79768986997783,1.,-0.761229695230558));
#33744=CARTESIAN_POINT('Ctrl Pts',(1.7918581561088,1.,-0.760469555880749));
#33745=CARTESIAN_POINT('Ctrl Pts',(1.78596964884604,1.,-0.75961440111019));
#33746=CARTESIAN_POINT('Ctrl Pts',(1.77999411220945,1.,-0.758650626677519));
#33747=CARTESIAN_POINT('Ctrl Pts',(1.77394167108292,1.,-0.757578264077029));
#33748=CARTESIAN_POINT('Ctrl Pts',(1.76789396002998,1.,-0.75642189602781));
#33749=CARTESIAN_POINT('Ctrl Pts',(1.76197817240128,1.,-0.755220979974462));
#33750=CARTESIAN_POINT('Ctrl Pts',(1.75631083600019,1.,-0.754009254027829));
#33751=CARTESIAN_POINT('Ctrl Pts',(1.75095139468794,1.,-0.752797683531314));
#33752=CARTESIAN_POINT('Ctrl Pts',(1.74585086852502,1.,-0.751555614164483));
#33753=CARTESIAN_POINT('Ctrl Pts',(1.74080458267114,1.,-0.75019343598125));
#33754=CARTESIAN_POINT('Ctrl Pts',(1.7355035168033,1.,-0.74858246295687));
#33755=CARTESIAN_POINT('Ctrl Pts',(1.72958533647714,1.,-0.746574710097752));
#33756=CARTESIAN_POINT('Ctrl Pts',(1.72268229916769,1.,-0.744021445433094));
#33757=CARTESIAN_POINT('Ctrl Pts',(1.71447789751001,1.,-0.74079516202821));
#33758=CARTESIAN_POINT('Ctrl Pts',(1.70473309004249,1.,-0.736799665716932));
#33759=CARTESIAN_POINT('Ctrl Pts',(1.69326921972915,1.,-0.731963238685357));
#33760=CARTESIAN_POINT('Ctrl Pts',(1.67996158451922,1.,-0.726235967982445));
#33761=CARTESIAN_POINT('Ctrl Pts',(1.66472880551777,1.,-0.71958543378795));
#33762=CARTESIAN_POINT('Ctrl Pts',(1.64752408828442,1.,-0.711993139340448));
#33763=CARTESIAN_POINT('Ctrl Pts',(1.6321654166204,1.,-0.705159151977294));
#33764=CARTESIAN_POINT('Ctrl Pts',(1.61974673471117,1.,-0.699605146398837));
#33765=CARTESIAN_POINT('Ctrl Pts',(1.61106790957619,1.,-0.69571209787897));
#33766=CARTESIAN_POINT('Ctrl Pts',(1.60662857109684,1.,-0.693717979106306));
#33767=CARTESIAN_POINT('',(2.0698113262342,0.,-0.745574324794401));
#33768=CARTESIAN_POINT('Origin',(2.11275013067528,0.,-0.61342227326009));
#33769=CARTESIAN_POINT('',(2.11275013067528,1.,-0.61342227326009));
#33770=CARTESIAN_POINT('',(2.0698113262342,1.,-0.745574324794401));
#33771=CARTESIAN_POINT('',(2.11275013067528,0.,-0.61342227326009));
#33772=CARTESIAN_POINT('Ctrl Pts',(1.7075470150345,-1.,-0.383122945602004));
#33773=CARTESIAN_POINT('Ctrl Pts',(1.7075470150345,1.,-0.383122945602004));
#33774=CARTESIAN_POINT('Ctrl Pts',(1.71231062891958,-1.,-0.384119047315542));
#33775=CARTESIAN_POINT('Ctrl Pts',(1.71231062891958,1.,-0.384119047315542));
#33776=CARTESIAN_POINT('Ctrl Pts',(1.72162022246158,-1.,-0.38607079032701));
#33777=CARTESIAN_POINT('Ctrl Pts',(1.72162022246158,1.,-0.38607079032701));
#33778=CARTESIAN_POINT('Ctrl Pts',(1.7349317097561,-1.,-0.388877023509192));
#33779=CARTESIAN_POINT('Ctrl Pts',(1.7349317097561,1.,-0.388877023509192));
#33780=CARTESIAN_POINT('Ctrl Pts',(1.75137405313962,-1.,-0.392375812294307));
#33781=CARTESIAN_POINT('Ctrl Pts',(1.75137405313962,1.,-0.392375812294307));
#33782=CARTESIAN_POINT('Ctrl Pts',(1.7697556004756,-1.,-0.39634619612042));
#33783=CARTESIAN_POINT('Ctrl Pts',(1.7697556004756,1.,-0.39634619612042));
#33784=CARTESIAN_POINT('Ctrl Pts',(1.78598826347533,-1.,-0.399919403783081));
#33785=CARTESIAN_POINT('Ctrl Pts',(1.78598826347533,1.,-0.399919403783081));
#33786=CARTESIAN_POINT('Ctrl Pts',(1.80012077176221,-1.,-0.403107976170441));
#33787=CARTESIAN_POINT('Ctrl Pts',(1.80012077176221,1.,-0.403107976170441));
#33788=CARTESIAN_POINT('Ctrl Pts',(1.81223801813988,-1.,-0.405933518411838));
#33789=CARTESIAN_POINT('Ctrl Pts',(1.81223801813988,1.,-0.405933518411838));
#33790=CARTESIAN_POINT('Ctrl Pts',(1.8224702267854,-1.,-0.408428948108534));
#33791=CARTESIAN_POINT('Ctrl Pts',(1.8224702267854,1.,-0.408428948108534));
#33792=CARTESIAN_POINT('Ctrl Pts',(1.83100408895216,-1.,-0.410641256301675));
#33793=CARTESIAN_POINT('Ctrl Pts',(1.83100408895216,1.,-0.410641256301675));
#33794=CARTESIAN_POINT('Ctrl Pts',(1.83808953475839,-1.,-0.412633125322162));
#33795=CARTESIAN_POINT('Ctrl Pts',(1.83808953475839,1.,-0.412633125322162));
#33796=CARTESIAN_POINT('Ctrl Pts',(1.8440575707371,-1.,-0.41448743825434));
#33797=CARTESIAN_POINT('Ctrl Pts',(1.8440575707371,1.,-0.41448743825434));
#33798=CARTESIAN_POINT('Ctrl Pts',(1.84929312929882,-1.,-0.416300022038864));
#33799=CARTESIAN_POINT('Ctrl Pts',(1.84929312929882,1.,-0.416300022038864));
#33800=CARTESIAN_POINT('Ctrl Pts',(1.85417632856234,-1.,-0.418164129143534));
#33801=CARTESIAN_POINT('Ctrl Pts',(1.85417632856234,1.,-0.418164129143534));
#33802=CARTESIAN_POINT('Ctrl Pts',(1.85903281096686,-1.,-0.42015728797562));
#33803=CARTESIAN_POINT('Ctrl Pts',(1.85903281096686,1.,-0.42015728797562));
#33804=CARTESIAN_POINT('Ctrl Pts',(1.86408083334028,-1.,-0.422327307418275));
#33805=CARTESIAN_POINT('Ctrl Pts',(1.86408083334028,1.,-0.422327307418275));
#33806=CARTESIAN_POINT('Ctrl Pts',(1.86937803944323,-1.,-0.424678177291359));
#33807=CARTESIAN_POINT('Ctrl Pts',(1.86937803944323,1.,-0.424678177291359));
#33808=CARTESIAN_POINT('Ctrl Pts',(1.87486989291484,-1.,-0.427183828519102));
#33809=CARTESIAN_POINT('Ctrl Pts',(1.87486989291484,1.,-0.427183828519102));
#33810=CARTESIAN_POINT('Ctrl Pts',(1.88044229001832,-1.,-0.429803062482345));
#33811=CARTESIAN_POINT('Ctrl Pts',(1.88044229001832,1.,-0.429803062482345));
#33812=CARTESIAN_POINT('Ctrl Pts',(1.88596913666793,-1.,-0.432493038548748));
#33813=CARTESIAN_POINT('Ctrl Pts',(1.88596913666793,1.,-0.432493038548748));
#33814=CARTESIAN_POINT('Ctrl Pts',(1.89136993975504,-1.,-0.435225660963383));
#33815=CARTESIAN_POINT('Ctrl Pts',(1.89136993975504,1.,-0.435225660963383));
#33816=CARTESIAN_POINT('Ctrl Pts',(1.89663648956466,-1.,-0.437995003948244));
#33817=CARTESIAN_POINT('Ctrl Pts',(1.89663648956466,1.,-0.437995003948244));
#33818=CARTESIAN_POINT('Ctrl Pts',(1.90180124389086,-1.,-0.440807833704038));
#33819=CARTESIAN_POINT('Ctrl Pts',(1.90180124389086,1.,-0.440807833704038));
#33820=CARTESIAN_POINT('Ctrl Pts',(1.90691756144898,-1.,-0.443677556849151));
#33821=CARTESIAN_POINT('Ctrl Pts',(1.90691756144898,1.,-0.443677556849151));
#33822=CARTESIAN_POINT('Ctrl Pts',(1.9120369998112,-1.,-0.446617343485711));
#33823=CARTESIAN_POINT('Ctrl Pts',(1.9120369998112,1.,-0.446617343485711));
#33824=CARTESIAN_POINT('Ctrl Pts',(1.91718342555755,-1.,-0.449632260106662));
#33825=CARTESIAN_POINT('Ctrl Pts',(1.91718342555755,1.,-0.449632260106662));
#33826=CARTESIAN_POINT('Ctrl Pts',(1.92235380648502,-1.,-0.452719478359433));
#33827=CARTESIAN_POINT('Ctrl Pts',(1.92235380648502,1.,-0.452719478359433));
#33828=CARTESIAN_POINT('Ctrl Pts',(1.92753067150476,-1.,-0.455872005174371));
#33829=CARTESIAN_POINT('Ctrl Pts',(1.92753067150476,1.,-0.455872005174371));
#33830=CARTESIAN_POINT('Ctrl Pts',(1.93269066517934,-1.,-0.459081234547926));
#33831=CARTESIAN_POINT('Ctrl Pts',(1.93269066517934,1.,-0.459081234547926));
#33832=CARTESIAN_POINT('Ctrl Pts',(1.93781486640821,-1.,-0.462340031009057));
#33833=CARTESIAN_POINT('Ctrl Pts',(1.93781486640821,1.,-0.462340031009057));
#33834=CARTESIAN_POINT('Ctrl Pts',(1.9428979419619,-1.,-0.46564546202603));
#33835=CARTESIAN_POINT('Ctrl Pts',(1.9428979419619,1.,-0.46564546202603));
#33836=CARTESIAN_POINT('Ctrl Pts',(1.94794381136514,-1.,-0.468997482913135));
#33837=CARTESIAN_POINT('Ctrl Pts',(1.94794381136514,1.,-0.468997482913135));
#33838=CARTESIAN_POINT('Ctrl Pts',(1.95296148278133,-1.,-0.472397672264072));
#33839=CARTESIAN_POINT('Ctrl Pts',(1.95296148278133,1.,-0.472397672264072));
#33840=CARTESIAN_POINT('Ctrl Pts',(1.95796111148177,-1.,-0.475848034683176));
#33841=CARTESIAN_POINT('Ctrl Pts',(1.95796111148177,1.,-0.475848034683176));
#33842=CARTESIAN_POINT('Ctrl Pts',(1.96294933055943,-1.,-0.479349583074855));
#33843=CARTESIAN_POINT('Ctrl Pts',(1.96294933055943,1.,-0.479349583074855));
#33844=CARTESIAN_POINT('Ctrl Pts',(1.96792703422362,-1.,-0.482901662120691));
#33845=CARTESIAN_POINT('Ctrl Pts',(1.96792703422362,1.,-0.482901662120691));
#33846=CARTESIAN_POINT('Ctrl Pts',(1.97289186263272,-1.,-0.486502692907659));
#33847=CARTESIAN_POINT('Ctrl Pts',(1.97289186263272,1.,-0.486502692907659));
#33848=CARTESIAN_POINT('Ctrl Pts',(1.97783973019229,-1.,-0.490150627860953));
#33849=CARTESIAN_POINT('Ctrl Pts',(1.97783973019229,1.,-0.490150627860953));
#33850=CARTESIAN_POINT('Ctrl Pts',(1.98276658761821,-1.,-0.493843476541495));
#33851=CARTESIAN_POINT('Ctrl Pts',(1.98276658761821,1.,-0.493843476541495));
#33852=CARTESIAN_POINT('Ctrl Pts',(1.98767044752932,-1.,-0.497579909545574));
#33853=CARTESIAN_POINT('Ctrl Pts',(1.98767044752932,1.,-0.497579909545574));
#33854=CARTESIAN_POINT('Ctrl Pts',(1.99255149126155,-1.,-0.501359287727146));
#33855=CARTESIAN_POINT('Ctrl Pts',(1.99255149126155,1.,-0.501359287727146));
#33856=CARTESIAN_POINT('Ctrl Pts',(1.99741107463572,-1.,-0.505181361323026));
#33857=CARTESIAN_POINT('Ctrl Pts',(1.99741107463572,1.,-0.505181361323026));
#33858=CARTESIAN_POINT('Ctrl Pts',(2.00225107134734,-1.,-0.509046069886157));
#33859=CARTESIAN_POINT('Ctrl Pts',(2.00225107134734,1.,-0.509046069886157));
#33860=CARTESIAN_POINT('Ctrl Pts',(2.00707309946949,-1.,-0.512953306961793));
#33861=CARTESIAN_POINT('Ctrl Pts',(2.00707309946949,1.,-0.512953306961793));
#33862=CARTESIAN_POINT('Ctrl Pts',(2.01187773939242,-1.,-0.516902681728687));
#33863=CARTESIAN_POINT('Ctrl Pts',(2.01187773939242,1.,-0.516902681728687));
#33864=CARTESIAN_POINT('Ctrl Pts',(2.01666477917286,-1.,-0.520893590399371));
#33865=CARTESIAN_POINT('Ctrl Pts',(2.01666477917286,1.,-0.520893590399371));
#33866=CARTESIAN_POINT('Ctrl Pts',(2.02143356304698,-1.,-0.524925318333476));
#33867=CARTESIAN_POINT('Ctrl Pts',(2.02143356304698,1.,-0.524925318333476));
#33868=CARTESIAN_POINT('Ctrl Pts',(2.0261832908329,-1.,-0.528997127241914));
#33869=CARTESIAN_POINT('Ctrl Pts',(2.0261832908329,1.,-0.528997127241914));
#33870=CARTESIAN_POINT('Ctrl Pts',(2.03091336214426,-1.,-0.533108355132977));
#33871=CARTESIAN_POINT('Ctrl Pts',(2.03091336214426,1.,-0.533108355132977));
#33872=CARTESIAN_POINT('Ctrl Pts',(2.03562362954037,-1.,-0.537258489833262));
#33873=CARTESIAN_POINT('Ctrl Pts',(2.03562362954037,1.,-0.537258489833262));
#33874=CARTESIAN_POINT('Ctrl Pts',(2.04031422690527,-1.,-0.541447120615659));
#33875=CARTESIAN_POINT('Ctrl Pts',(2.04031422690527,1.,-0.541447120615659));
#33876=CARTESIAN_POINT('Ctrl Pts',(2.04498544714588,-1.,-0.54567390381743));
#33877=CARTESIAN_POINT('Ctrl Pts',(2.04498544714588,1.,-0.54567390381743));
#33878=CARTESIAN_POINT('Ctrl Pts',(2.04963761077958,-1.,-0.549938525150295));
#33879=CARTESIAN_POINT('Ctrl Pts',(2.04963761077958,1.,-0.549938525150295));
#33880=CARTESIAN_POINT('Ctrl Pts',(2.05427091604413,-1.,-0.554240657463906));
#33881=CARTESIAN_POINT('Ctrl Pts',(2.05427091604413,1.,-0.554240657463906));
#33882=CARTESIAN_POINT('Ctrl Pts',(2.05888537756462,-1.,-0.558579940185152));
#33883=CARTESIAN_POINT('Ctrl Pts',(2.05888537756462,1.,-0.558579940185152));
#33884=CARTESIAN_POINT('Ctrl Pts',(2.06348090160589,-1.,-0.562955993082262));
#33885=CARTESIAN_POINT('Ctrl Pts',(2.06348090160589,1.,-0.562955993082262));
#33886=CARTESIAN_POINT('Ctrl Pts',(2.06805732997334,-1.,-0.567368421181087));
#33887=CARTESIAN_POINT('Ctrl Pts',(2.06805732997334,1.,-0.567368421181087));
#33888=CARTESIAN_POINT('Ctrl Pts',(2.07261449292824,-1.,-0.571816823242603));
#33889=CARTESIAN_POINT('Ctrl Pts',(2.07261449292824,1.,-0.571816823242603));
#33890=CARTESIAN_POINT('Ctrl Pts',(2.07715226767559,-1.,-0.576300797416845));
#33891=CARTESIAN_POINT('Ctrl Pts',(2.07715226767559,1.,-0.576300797416845));
#33892=CARTESIAN_POINT('Ctrl Pts',(2.08167059018418,-1.,-0.580819952108064));
#33893=CARTESIAN_POINT('Ctrl Pts',(2.08167059018418,1.,-0.580819952108064));
#33894=CARTESIAN_POINT('Ctrl Pts',(2.08616943727951,-1.,-0.585373918991617));
#33895=CARTESIAN_POINT('Ctrl Pts',(2.08616943727951,1.,-0.585373918991617));
#33896=CARTESIAN_POINT('Ctrl Pts',(2.09064881812129,-1.,-0.589962365403406));
#33897=CARTESIAN_POINT('Ctrl Pts',(2.09064881812129,1.,-0.589962365403406));
#33898=CARTESIAN_POINT('Ctrl Pts',(2.0951087622027,-1.,-0.594585006052162));
#33899=CARTESIAN_POINT('Ctrl Pts',(2.0951087622027,1.,-0.594585006052162));
#33900=CARTESIAN_POINT('Ctrl Pts',(2.0995493086477,-1.,-0.599241616420534));
#33901=CARTESIAN_POINT('Ctrl Pts',(2.0995493086477,1.,-0.599241616420534));
#33902=CARTESIAN_POINT('Ctrl Pts',(2.10397049886949,-1.,-0.60393203073603));
#33903=CARTESIAN_POINT('Ctrl Pts',(2.10397049886949,1.,-0.60393203073603));
#33904=CARTESIAN_POINT('Ctrl Pts',(2.1074919961518,-1.,-0.607711315454876));
#33905=CARTESIAN_POINT('Ctrl Pts',(2.1074919961518,1.,-0.607711315454876));
#33906=CARTESIAN_POINT('Ctrl Pts',(2.11012443807238,-1.,-0.610560911689899));
#33907=CARTESIAN_POINT('Ctrl Pts',(2.11012443807238,1.,-0.610560911689899));
#33908=CARTESIAN_POINT('Ctrl Pts',(2.11187554259986,-1.,-0.6124673655618));
#33909=CARTESIAN_POINT('Ctrl Pts',(2.11187554259986,1.,-0.6124673655618));
#33910=CARTESIAN_POINT('Ctrl Pts',(2.11275013067528,-1.,-0.61342227326009));
#33911=CARTESIAN_POINT('Ctrl Pts',(2.11275013067528,1.,-0.61342227326009));
#33912=CARTESIAN_POINT('',(1.7075470150345,1.,-0.383122945602004));
#33913=CARTESIAN_POINT('Ctrl Pts',(1.7075470150345,1.,-0.383122945602004));
#33914=CARTESIAN_POINT('Ctrl Pts',(1.71231062891958,1.,-0.384119047315542));
#33915=CARTESIAN_POINT('Ctrl Pts',(1.72162022246158,1.,-0.38607079032701));
#33916=CARTESIAN_POINT('Ctrl Pts',(1.7349317097561,1.,-0.388877023509192));
#33917=CARTESIAN_POINT('Ctrl Pts',(1.75137405313962,1.,-0.392375812294307));
#33918=CARTESIAN_POINT('Ctrl Pts',(1.7697556004756,1.,-0.39634619612042));
#33919=CARTESIAN_POINT('Ctrl Pts',(1.78598826347533,1.,-0.399919403783081));
#33920=CARTESIAN_POINT('Ctrl Pts',(1.80012077176221,1.,-0.403107976170441));
#33921=CARTESIAN_POINT('Ctrl Pts',(1.81223801813988,1.,-0.405933518411838));
#33922=CARTESIAN_POINT('Ctrl Pts',(1.8224702267854,1.,-0.408428948108534));
#33923=CARTESIAN_POINT('Ctrl Pts',(1.83100408895216,1.,-0.410641256301675));
#33924=CARTESIAN_POINT('Ctrl Pts',(1.83808953475839,1.,-0.412633125322162));
#33925=CARTESIAN_POINT('Ctrl Pts',(1.8440575707371,1.,-0.41448743825434));
#33926=CARTESIAN_POINT('Ctrl Pts',(1.84929312929882,1.,-0.416300022038864));
#33927=CARTESIAN_POINT('Ctrl Pts',(1.85417632856234,1.,-0.418164129143534));
#33928=CARTESIAN_POINT('Ctrl Pts',(1.85903281096686,1.,-0.42015728797562));
#33929=CARTESIAN_POINT('Ctrl Pts',(1.86408083334028,1.,-0.422327307418275));
#33930=CARTESIAN_POINT('Ctrl Pts',(1.86937803944323,1.,-0.424678177291359));
#33931=CARTESIAN_POINT('Ctrl Pts',(1.87486989291484,1.,-0.427183828519102));
#33932=CARTESIAN_POINT('Ctrl Pts',(1.88044229001832,1.,-0.429803062482345));
#33933=CARTESIAN_POINT('Ctrl Pts',(1.88596913666793,1.,-0.432493038548748));
#33934=CARTESIAN_POINT('Ctrl Pts',(1.89136993975504,1.,-0.435225660963383));
#33935=CARTESIAN_POINT('Ctrl Pts',(1.89663648956466,1.,-0.437995003948244));
#33936=CARTESIAN_POINT('Ctrl Pts',(1.90180124389086,1.,-0.440807833704038));
#33937=CARTESIAN_POINT('Ctrl Pts',(1.90691756144898,1.,-0.443677556849151));
#33938=CARTESIAN_POINT('Ctrl Pts',(1.9120369998112,1.,-0.446617343485711));
#33939=CARTESIAN_POINT('Ctrl Pts',(1.91718342555755,1.,-0.449632260106662));
#33940=CARTESIAN_POINT('Ctrl Pts',(1.92235380648502,1.,-0.452719478359433));
#33941=CARTESIAN_POINT('Ctrl Pts',(1.92753067150476,1.,-0.455872005174371));
#33942=CARTESIAN_POINT('Ctrl Pts',(1.93269066517934,1.,-0.459081234547926));
#33943=CARTESIAN_POINT('Ctrl Pts',(1.93781486640821,1.,-0.462340031009057));
#33944=CARTESIAN_POINT('Ctrl Pts',(1.9428979419619,1.,-0.46564546202603));
#33945=CARTESIAN_POINT('Ctrl Pts',(1.94794381136514,1.,-0.468997482913135));
#33946=CARTESIAN_POINT('Ctrl Pts',(1.95296148278133,1.,-0.472397672264072));
#33947=CARTESIAN_POINT('Ctrl Pts',(1.95796111148177,1.,-0.475848034683176));
#33948=CARTESIAN_POINT('Ctrl Pts',(1.96294933055943,1.,-0.479349583074855));
#33949=CARTESIAN_POINT('Ctrl Pts',(1.96792703422362,1.,-0.482901662120691));
#33950=CARTESIAN_POINT('Ctrl Pts',(1.97289186263272,1.,-0.486502692907659));
#33951=CARTESIAN_POINT('Ctrl Pts',(1.97783973019229,1.,-0.490150627860953));
#33952=CARTESIAN_POINT('Ctrl Pts',(1.98276658761821,1.,-0.493843476541495));
#33953=CARTESIAN_POINT('Ctrl Pts',(1.98767044752932,1.,-0.497579909545574));
#33954=CARTESIAN_POINT('Ctrl Pts',(1.99255149126155,1.,-0.501359287727146));
#33955=CARTESIAN_POINT('Ctrl Pts',(1.99741107463572,1.,-0.505181361323026));
#33956=CARTESIAN_POINT('Ctrl Pts',(2.00225107134734,1.,-0.509046069886157));
#33957=CARTESIAN_POINT('Ctrl Pts',(2.00707309946949,1.,-0.512953306961793));
#33958=CARTESIAN_POINT('Ctrl Pts',(2.01187773939242,1.,-0.516902681728687));
#33959=CARTESIAN_POINT('Ctrl Pts',(2.01666477917286,1.,-0.520893590399371));
#33960=CARTESIAN_POINT('Ctrl Pts',(2.02143356304698,1.,-0.524925318333476));
#33961=CARTESIAN_POINT('Ctrl Pts',(2.0261832908329,1.,-0.528997127241914));
#33962=CARTESIAN_POINT('Ctrl Pts',(2.03091336214426,1.,-0.533108355132977));
#33963=CARTESIAN_POINT('Ctrl Pts',(2.03562362954037,1.,-0.537258489833262));
#33964=CARTESIAN_POINT('Ctrl Pts',(2.04031422690527,1.,-0.541447120615659));
#33965=CARTESIAN_POINT('Ctrl Pts',(2.04498544714588,1.,-0.54567390381743));
#33966=CARTESIAN_POINT('Ctrl Pts',(2.04963761077958,1.,-0.549938525150295));
#33967=CARTESIAN_POINT('Ctrl Pts',(2.05427091604413,1.,-0.554240657463906));
#33968=CARTESIAN_POINT('Ctrl Pts',(2.05888537756462,1.,-0.558579940185152));
#33969=CARTESIAN_POINT('Ctrl Pts',(2.06348090160589,1.,-0.562955993082262));
#33970=CARTESIAN_POINT('Ctrl Pts',(2.06805732997334,1.,-0.567368421181087));
#33971=CARTESIAN_POINT('Ctrl Pts',(2.07261449292824,1.,-0.571816823242603));
#33972=CARTESIAN_POINT('Ctrl Pts',(2.07715226767559,1.,-0.576300797416845));
#33973=CARTESIAN_POINT('Ctrl Pts',(2.08167059018418,1.,-0.580819952108064));
#33974=CARTESIAN_POINT('Ctrl Pts',(2.08616943727951,1.,-0.585373918991617));
#33975=CARTESIAN_POINT('Ctrl Pts',(2.09064881812129,1.,-0.589962365403406));
#33976=CARTESIAN_POINT('Ctrl Pts',(2.0951087622027,1.,-0.594585006052162));
#33977=CARTESIAN_POINT('Ctrl Pts',(2.0995493086477,1.,-0.599241616420534));
#33978=CARTESIAN_POINT('Ctrl Pts',(2.10397049886949,1.,-0.60393203073603));
#33979=CARTESIAN_POINT('Ctrl Pts',(2.1074919961518,1.,-0.607711315454876));
#33980=CARTESIAN_POINT('Ctrl Pts',(2.11012443807238,1.,-0.610560911689899));
#33981=CARTESIAN_POINT('Ctrl Pts',(2.11187554259986,1.,-0.6124673655618));
#33982=CARTESIAN_POINT('Ctrl Pts',(2.11275013067528,1.,-0.61342227326009));
#33983=CARTESIAN_POINT('',(1.7075470150345,0.,-0.383122945602001));
#33984=CARTESIAN_POINT('Origin',(0.,0.,0.));
#33985=CARTESIAN_POINT('',(1.74236521665491,1.,-0.163289472382896));
#33986=CARTESIAN_POINT('Origin',(0.,1.,0.));
#33987=CARTESIAN_POINT('',(1.74236521665491,0.,-0.163289472382896));
#33988=CARTESIAN_POINT('Ctrl Pts',(2.19890268624765,-1.,-0.0694764450219582));
#33989=CARTESIAN_POINT('Ctrl Pts',(2.19890268624765,1.,-0.0694764450219582));
#33990=CARTESIAN_POINT('Ctrl Pts',(2.19777582085423,-1.,-0.0701143536325491));
#33991=CARTESIAN_POINT('Ctrl Pts',(2.19777582085423,1.,-0.0701143536325491));
#33992=CARTESIAN_POINT('Ctrl Pts',(2.19552129484002,-1.,-0.0713863779526155));
#33993=CARTESIAN_POINT('Ctrl Pts',(2.19552129484002,1.,-0.0713863779526155));
#33994=CARTESIAN_POINT('Ctrl Pts',(2.19213712013662,-1.,-0.0732830357306726));
#33995=CARTESIAN_POINT('Ctrl Pts',(2.19213712013662,1.,-0.0732830357306726));
#33996=CARTESIAN_POINT('Ctrl Pts',(2.1876201139953,-1.,-0.0757891465836149));
#33997=CARTESIAN_POINT('Ctrl Pts',(2.1876201139953,1.,-0.0757891465836149));
#33998=CARTESIAN_POINT('Ctrl Pts',(2.18196589448887,-1.,-0.0788837727685244));
#33999=CARTESIAN_POINT('Ctrl Pts',(2.18196589448887,1.,-0.0788837727685244));
#34000=CARTESIAN_POINT('Ctrl Pts',(2.176303712113,-1.,-0.0819402680872767));
#34001=CARTESIAN_POINT('Ctrl Pts',(2.176303712113,1.,-0.0819402680872767));
#34002=CARTESIAN_POINT('Ctrl Pts',(2.17063357870952,-1.,-0.0849584620835374));
#34003=CARTESIAN_POINT('Ctrl Pts',(2.17063357870952,1.,-0.0849584620835374));
#34004=CARTESIAN_POINT('Ctrl Pts',(2.16495552645014,-1.,-0.0879381291386924));
#34005=CARTESIAN_POINT('Ctrl Pts',(2.16495552645014,1.,-0.0879381291386924));
#34006=CARTESIAN_POINT('Ctrl Pts',(2.15926961544516,-1.,-0.0908789888107267));
#34007=CARTESIAN_POINT('Ctrl Pts',(2.15926961544516,1.,-0.0908789888107267));
#34008=CARTESIAN_POINT('Ctrl Pts',(2.1535759397817,-1.,-0.0937807218867645));
#34009=CARTESIAN_POINT('Ctrl Pts',(2.1535759397817,1.,-0.0937807218867645));
#34010=CARTESIAN_POINT('Ctrl Pts',(2.14787463531795,-1.,-0.096642985230546));
#34011=CARTESIAN_POINT('Ctrl Pts',(2.14787463531795,1.,-0.096642985230546));
#34012=CARTESIAN_POINT('Ctrl Pts',(2.14216588396025,-1.,-0.0994654261990917));
#34013=CARTESIAN_POINT('Ctrl Pts',(2.14216588396025,1.,-0.0994654261990917));
#34014=CARTESIAN_POINT('Ctrl Pts',(2.13644992667165,-1.,-0.102247700556101));
#34015=CARTESIAN_POINT('Ctrl Pts',(2.13644992667165,1.,-0.102247700556101));
#34016=CARTESIAN_POINT('Ctrl Pts',(2.13072704887293,-1.,-0.10498947915274));
#34017=CARTESIAN_POINT('Ctrl Pts',(2.13072704887293,1.,-0.10498947915274));
#34018=CARTESIAN_POINT('Ctrl Pts',(2.12499752307,-1.,-0.10769043523109));
#34019=CARTESIAN_POINT('Ctrl Pts',(2.12499752307,1.,-0.10769043523109));
#34020=CARTESIAN_POINT('Ctrl Pts',(2.11926155590865,-1.,-0.110350236135025));
#34021=CARTESIAN_POINT('Ctrl Pts',(2.11926155590865,1.,-0.110350236135025));
#34022=CARTESIAN_POINT('Ctrl Pts',(2.11351924490306,-1.,-0.112968534419737));
#34023=CARTESIAN_POINT('Ctrl Pts',(2.11351924490306,1.,-0.112968534419737));
#34024=CARTESIAN_POINT('Ctrl Pts',(2.10777050261309,-1.,-0.115544957687927));
#34025=CARTESIAN_POINT('Ctrl Pts',(2.10777050261309,1.,-0.115544957687927));
#34026=CARTESIAN_POINT('Ctrl Pts',(2.102015121329,-1.,-0.118079107988356));
#34027=CARTESIAN_POINT('Ctrl Pts',(2.102015121329,1.,-0.118079107988356));
#34028=CARTESIAN_POINT('Ctrl Pts',(2.0962529286773,-1.,-0.120570567965122));
#34029=CARTESIAN_POINT('Ctrl Pts',(2.0962529286773,1.,-0.120570567965122));
#34030=CARTESIAN_POINT('Ctrl Pts',(2.09048392424825,-1.,-0.123018905621083));
#34031=CARTESIAN_POINT('Ctrl Pts',(2.09048392424825,1.,-0.123018905621083));
#34032=CARTESIAN_POINT('Ctrl Pts',(2.08470840653643,-1.,-0.125423679412062));
#34033=CARTESIAN_POINT('Ctrl Pts',(2.08470840653643,1.,-0.125423679412062));
#34034=CARTESIAN_POINT('Ctrl Pts',(2.07892715110987,-1.,-0.12778444527612));
#34035=CARTESIAN_POINT('Ctrl Pts',(2.07892715110987,1.,-0.12778444527612));
#34036=CARTESIAN_POINT('Ctrl Pts',(2.07314114713063,-1.,-0.130100748328404));
#34037=CARTESIAN_POINT('Ctrl Pts',(2.07314114713063,1.,-0.130100748328404));
#34038=CARTESIAN_POINT('Ctrl Pts',(2.06735123910326,-1.,-0.132372111547711));
#34039=CARTESIAN_POINT('Ctrl Pts',(2.06735123910326,1.,-0.132372111547711));
#34040=CARTESIAN_POINT('Ctrl Pts',(2.06155781517842,-1.,-0.134598026192106));
#34041=CARTESIAN_POINT('Ctrl Pts',(2.06155781517842,1.,-0.134598026192106));
#34042=CARTESIAN_POINT('Ctrl Pts',(2.05576044414264,-1.,-0.136777941218044));
#34043=CARTESIAN_POINT('Ctrl Pts',(2.05576044414264,1.,-0.136777941218044));
#34044=CARTESIAN_POINT('Ctrl Pts',(2.04995762001328,-1.,-0.138911255368966));
#34045=CARTESIAN_POINT('Ctrl Pts',(2.04995762001328,1.,-0.138911255368966));
#34046=CARTESIAN_POINT('Ctrl Pts',(2.04414757947916,-1.,-0.140997332152546));
#34047=CARTESIAN_POINT('Ctrl Pts',(2.04414757947916,1.,-0.140997332152546));
#34048=CARTESIAN_POINT('Ctrl Pts',(2.03832911025912,-1.,-0.143035515058209));
#34049=CARTESIAN_POINT('Ctrl Pts',(2.03832911025912,1.,-0.143035515058209));
#34050=CARTESIAN_POINT('Ctrl Pts',(2.03250223739942,-1.,-0.145025140186058));
#34051=CARTESIAN_POINT('Ctrl Pts',(2.03250223739942,1.,-0.145025140186058));
#34052=CARTESIAN_POINT('Ctrl Pts',(2.02666926182017,-1.,-0.146965557332583));
#34053=CARTESIAN_POINT('Ctrl Pts',(2.02666926182017,1.,-0.146965557332583));
#34054=CARTESIAN_POINT('Ctrl Pts',(2.02083464969894,-1.,-0.148856124775337));
#34055=CARTESIAN_POINT('Ctrl Pts',(2.02083464969894,1.,-0.148856124775337));
#34056=CARTESIAN_POINT('Ctrl Pts',(2.01500291940238,-1.,-0.150696157673078));
#34057=CARTESIAN_POINT('Ctrl Pts',(2.01500291940238,1.,-0.150696157673078));
#34058=CARTESIAN_POINT('Ctrl Pts',(2.00917680318424,-1.,-0.15248488362145));
#34059=CARTESIAN_POINT('Ctrl Pts',(2.00917680318424,1.,-0.15248488362145));
#34060=CARTESIAN_POINT('Ctrl Pts',(2.00335565310543,-1.,-0.154221403049722));
#34061=CARTESIAN_POINT('Ctrl Pts',(2.00335565310543,1.,-0.154221403049722));
#34062=CARTESIAN_POINT('Ctrl Pts',(1.99753284771497,-1.,-0.155904629548784));
#34063=CARTESIAN_POINT('Ctrl Pts',(1.99753284771497,1.,-0.155904629548784));
#34064=CARTESIAN_POINT('Ctrl Pts',(1.99169810931908,-1.,-0.157533331459227));
#34065=CARTESIAN_POINT('Ctrl Pts',(1.99169810931908,1.,-0.157533331459227));
#34066=CARTESIAN_POINT('Ctrl Pts',(1.98584238283292,-1.,-0.159106226437299));
#34067=CARTESIAN_POINT('Ctrl Pts',(1.98584238283292,1.,-0.159106226437299));
#34068=CARTESIAN_POINT('Ctrl Pts',(1.97996195437559,-1.,-0.160622060784611));
#34069=CARTESIAN_POINT('Ctrl Pts',(1.97996195437559,1.,-0.160622060784611));
#34070=CARTESIAN_POINT('Ctrl Pts',(1.97406280235188,-1.,-0.162079693556289));
#34071=CARTESIAN_POINT('Ctrl Pts',(1.97406280235188,1.,-0.162079693556289));
#34072=CARTESIAN_POINT('Ctrl Pts',(1.96816512677967,-1.,-0.163478185457734));
#34073=CARTESIAN_POINT('Ctrl Pts',(1.96816512677967,1.,-0.163478185457734));
#34074=CARTESIAN_POINT('Ctrl Pts',(1.96229379940136,-1.,-0.164816568920269));
#34075=CARTESIAN_POINT('Ctrl Pts',(1.96229379940136,1.,-0.164816568920269));
#34076=CARTESIAN_POINT('Ctrl Pts',(1.9564675971873,-1.,-0.166093592002813));
#34077=CARTESIAN_POINT('Ctrl Pts',(1.9564675971873,1.,-0.166093592002813));
#34078=CARTESIAN_POINT('Ctrl Pts',(1.95069027794294,-1.,-0.167307501784476));
#34079=CARTESIAN_POINT('Ctrl Pts',(1.95069027794294,1.,-0.167307501784476));
#34080=CARTESIAN_POINT('Ctrl Pts',(1.94493757756931,-1.,-0.168455741607556));
#34081=CARTESIAN_POINT('Ctrl Pts',(1.94493757756931,1.,-0.168455741607556));
#34082=CARTESIAN_POINT('Ctrl Pts',(1.93915639211581,-1.,-0.169534904817491));
#34083=CARTESIAN_POINT('Ctrl Pts',(1.93915639211581,1.,-0.169534904817491));
#34084=CARTESIAN_POINT('Ctrl Pts',(1.93329183155539,-1.,-0.170541253116202));
#34085=CARTESIAN_POINT('Ctrl Pts',(1.93329183155539,1.,-0.170541253116202));
#34086=CARTESIAN_POINT('Ctrl Pts',(1.92731093582036,-1.,-0.171471191532988));
#34087=CARTESIAN_POINT('Ctrl Pts',(1.92731093582036,1.,-0.171471191532988));
#34088=CARTESIAN_POINT('Ctrl Pts',(1.9212233439798,-1.,-0.172321621259514));
#34089=CARTESIAN_POINT('Ctrl Pts',(1.9212233439798,1.,-0.172321621259514));
#34090=CARTESIAN_POINT('Ctrl Pts',(1.91511429159527,-1.,-0.173090695383496));
#34091=CARTESIAN_POINT('Ctrl Pts',(1.91511429159527,1.,-0.173090695383496));
#34092=CARTESIAN_POINT('Ctrl Pts',(1.90911693975267,-1.,-0.173776635257817));
#34093=CARTESIAN_POINT('Ctrl Pts',(1.90911693975267,1.,-0.173776635257817));
#34094=CARTESIAN_POINT('Ctrl Pts',(1.90335253862834,-1.,-0.174375518661085));
#34095=CARTESIAN_POINT('Ctrl Pts',(1.90335253862834,1.,-0.174375518661085));
#34096=CARTESIAN_POINT('Ctrl Pts',(1.89788101117132,-1.,-0.174879405091263));
#34097=CARTESIAN_POINT('Ctrl Pts',(1.89788101117132,1.,-0.174879405091263));
#34098=CARTESIAN_POINT('Ctrl Pts',(1.892646301985,-1.,-0.175274276190844));
#34099=CARTESIAN_POINT('Ctrl Pts',(1.892646301985,1.,-0.175274276190844));
#34100=CARTESIAN_POINT('Ctrl Pts',(1.88742606273259,-1.,-0.175538155840648));
#34101=CARTESIAN_POINT('Ctrl Pts',(1.88742606273259,1.,-0.175538155840648));
#34102=CARTESIAN_POINT('Ctrl Pts',(1.88188663145367,-1.,-0.175644148889699));
#34103=CARTESIAN_POINT('Ctrl Pts',(1.88188663145367,1.,-0.175644148889699));
#34104=CARTESIAN_POINT('Ctrl Pts',(1.87563767773588,-1.,-0.175563480746485));
#34105=CARTESIAN_POINT('Ctrl Pts',(1.87563767773588,1.,-0.175563480746485));
#34106=CARTESIAN_POINT('Ctrl Pts',(1.86828349694799,-1.,-0.175268337590758));
#34107=CARTESIAN_POINT('Ctrl Pts',(1.86828349694799,1.,-0.175268337590758));
#34108=CARTESIAN_POINT('Ctrl Pts',(1.85948367088837,-1.,-0.17473525927603));
#34109=CARTESIAN_POINT('Ctrl Pts',(1.85948367088837,1.,-0.17473525927603));
#34110=CARTESIAN_POINT('Ctrl Pts',(1.8489811319852,-1.,-0.173946627587732));
#34111=CARTESIAN_POINT('Ctrl Pts',(1.8489811319852,1.,-0.173946627587732));
#34112=CARTESIAN_POINT('Ctrl Pts',(1.83658380527692,-1.,-0.1728894428919));
#34113=CARTESIAN_POINT('Ctrl Pts',(1.83658380527692,1.,-0.1728894428919));
#34114=CARTESIAN_POINT('Ctrl Pts',(1.82215766811545,-1.,-0.171554770204119));
#34115=CARTESIAN_POINT('Ctrl Pts',(1.82215766811545,1.,-0.171554770204119));
#34116=CARTESIAN_POINT('Ctrl Pts',(1.80561530629706,-1.,-0.169936923904608));
#34117=CARTESIAN_POINT('Ctrl Pts',(1.80561530629706,1.,-0.169936923904608));
#34118=CARTESIAN_POINT('Ctrl Pts',(1.7869064998507,-1.,-0.168032772805197));
#34119=CARTESIAN_POINT('Ctrl Pts',(1.7869064998507,1.,-0.168032772805197));
#34120=CARTESIAN_POINT('Ctrl Pts',(1.77018771684844,-1.,-0.1662793551464));
#34121=CARTESIAN_POINT('Ctrl Pts',(1.77018771684844,1.,-0.1662793551464));
#34122=CARTESIAN_POINT('Ctrl Pts',(1.75666056638427,-1.,-0.164834765707159));
#34123=CARTESIAN_POINT('Ctrl Pts',(1.75666056638427,1.,-0.164834765707159));
#34124=CARTESIAN_POINT('Ctrl Pts',(1.7472034950333,-1.,-0.163814161002002));
#34125=CARTESIAN_POINT('Ctrl Pts',(1.7472034950333,1.,-0.163814161002002));
#34126=CARTESIAN_POINT('Ctrl Pts',(1.74236521665491,-1.,-0.163289472382896));
#34127=CARTESIAN_POINT('Ctrl Pts',(1.74236521665491,1.,-0.163289472382896));
#34128=CARTESIAN_POINT('',(2.19890268624765,1.,-0.0694764450219582));
#34129=CARTESIAN_POINT('Ctrl Pts',(2.19890268624765,1.,-0.0694764450219582));
#34130=CARTESIAN_POINT('Ctrl Pts',(2.19777582085423,1.,-0.0701143536325491));
#34131=CARTESIAN_POINT('Ctrl Pts',(2.19552129484002,1.,-0.0713863779526155));
#34132=CARTESIAN_POINT('Ctrl Pts',(2.19213712013662,1.,-0.0732830357306726));
#34133=CARTESIAN_POINT('Ctrl Pts',(2.1876201139953,1.,-0.0757891465836149));
#34134=CARTESIAN_POINT('Ctrl Pts',(2.18196589448887,1.,-0.0788837727685244));
#34135=CARTESIAN_POINT('Ctrl Pts',(2.176303712113,1.,-0.0819402680872767));
#34136=CARTESIAN_POINT('Ctrl Pts',(2.17063357870952,1.,-0.0849584620835374));
#34137=CARTESIAN_POINT('Ctrl Pts',(2.16495552645014,1.,-0.0879381291386924));
#34138=CARTESIAN_POINT('Ctrl Pts',(2.15926961544516,1.,-0.0908789888107267));
#34139=CARTESIAN_POINT('Ctrl Pts',(2.1535759397817,1.,-0.0937807218867645));
#34140=CARTESIAN_POINT('Ctrl Pts',(2.14787463531795,1.,-0.096642985230546));
#34141=CARTESIAN_POINT('Ctrl Pts',(2.14216588396025,1.,-0.0994654261990917));
#34142=CARTESIAN_POINT('Ctrl Pts',(2.13644992667165,1.,-0.102247700556101));
#34143=CARTESIAN_POINT('Ctrl Pts',(2.13072704887293,1.,-0.10498947915274));
#34144=CARTESIAN_POINT('Ctrl Pts',(2.12499752307,1.,-0.10769043523109));
#34145=CARTESIAN_POINT('Ctrl Pts',(2.11926155590865,1.,-0.110350236135025));
#34146=CARTESIAN_POINT('Ctrl Pts',(2.11351924490306,1.,-0.112968534419737));
#34147=CARTESIAN_POINT('Ctrl Pts',(2.10777050261309,1.,-0.115544957687927));
#34148=CARTESIAN_POINT('Ctrl Pts',(2.102015121329,1.,-0.118079107988356));
#34149=CARTESIAN_POINT('Ctrl Pts',(2.0962529286773,1.,-0.120570567965122));
#34150=CARTESIAN_POINT('Ctrl Pts',(2.09048392424825,1.,-0.123018905621083));
#34151=CARTESIAN_POINT('Ctrl Pts',(2.08470840653643,1.,-0.125423679412062));
#34152=CARTESIAN_POINT('Ctrl Pts',(2.07892715110987,1.,-0.12778444527612));
#34153=CARTESIAN_POINT('Ctrl Pts',(2.07314114713063,1.,-0.130100748328404));
#34154=CARTESIAN_POINT('Ctrl Pts',(2.06735123910326,1.,-0.132372111547711));
#34155=CARTESIAN_POINT('Ctrl Pts',(2.06155781517842,1.,-0.134598026192106));
#34156=CARTESIAN_POINT('Ctrl Pts',(2.05576044414264,1.,-0.136777941218044));
#34157=CARTESIAN_POINT('Ctrl Pts',(2.04995762001328,1.,-0.138911255368966));
#34158=CARTESIAN_POINT('Ctrl Pts',(2.04414757947916,1.,-0.140997332152546));
#34159=CARTESIAN_POINT('Ctrl Pts',(2.03832911025912,1.,-0.143035515058209));
#34160=CARTESIAN_POINT('Ctrl Pts',(2.03250223739942,1.,-0.145025140186058));
#34161=CARTESIAN_POINT('Ctrl Pts',(2.02666926182017,1.,-0.146965557332583));
#34162=CARTESIAN_POINT('Ctrl Pts',(2.02083464969894,1.,-0.148856124775337));
#34163=CARTESIAN_POINT('Ctrl Pts',(2.01500291940238,1.,-0.150696157673078));
#34164=CARTESIAN_POINT('Ctrl Pts',(2.00917680318424,1.,-0.15248488362145));
#34165=CARTESIAN_POINT('Ctrl Pts',(2.00335565310543,1.,-0.154221403049722));
#34166=CARTESIAN_POINT('Ctrl Pts',(1.99753284771497,1.,-0.155904629548784));
#34167=CARTESIAN_POINT('Ctrl Pts',(1.99169810931908,1.,-0.157533331459227));
#34168=CARTESIAN_POINT('Ctrl Pts',(1.98584238283292,1.,-0.159106226437299));
#34169=CARTESIAN_POINT('Ctrl Pts',(1.97996195437559,1.,-0.160622060784611));
#34170=CARTESIAN_POINT('Ctrl Pts',(1.97406280235188,1.,-0.162079693556289));
#34171=CARTESIAN_POINT('Ctrl Pts',(1.96816512677967,1.,-0.163478185457734));
#34172=CARTESIAN_POINT('Ctrl Pts',(1.96229379940136,1.,-0.164816568920269));
#34173=CARTESIAN_POINT('Ctrl Pts',(1.9564675971873,1.,-0.166093592002813));
#34174=CARTESIAN_POINT('Ctrl Pts',(1.95069027794294,1.,-0.167307501784476));
#34175=CARTESIAN_POINT('Ctrl Pts',(1.94493757756931,1.,-0.168455741607556));
#34176=CARTESIAN_POINT('Ctrl Pts',(1.93915639211581,1.,-0.169534904817491));
#34177=CARTESIAN_POINT('Ctrl Pts',(1.93329183155539,1.,-0.170541253116202));
#34178=CARTESIAN_POINT('Ctrl Pts',(1.92731093582036,1.,-0.171471191532988));
#34179=CARTESIAN_POINT('Ctrl Pts',(1.9212233439798,1.,-0.172321621259514));
#34180=CARTESIAN_POINT('Ctrl Pts',(1.91511429159527,1.,-0.173090695383496));
#34181=CARTESIAN_POINT('Ctrl Pts',(1.90911693975267,1.,-0.173776635257817));
#34182=CARTESIAN_POINT('Ctrl Pts',(1.90335253862834,1.,-0.174375518661085));
#34183=CARTESIAN_POINT('Ctrl Pts',(1.89788101117132,1.,-0.174879405091263));
#34184=CARTESIAN_POINT('Ctrl Pts',(1.892646301985,1.,-0.175274276190844));
#34185=CARTESIAN_POINT('Ctrl Pts',(1.88742606273259,1.,-0.175538155840648));
#34186=CARTESIAN_POINT('Ctrl Pts',(1.88188663145367,1.,-0.175644148889699));
#34187=CARTESIAN_POINT('Ctrl Pts',(1.87563767773588,1.,-0.175563480746485));
#34188=CARTESIAN_POINT('Ctrl Pts',(1.86828349694799,1.,-0.175268337590758));
#34189=CARTESIAN_POINT('Ctrl Pts',(1.85948367088837,1.,-0.17473525927603));
#34190=CARTESIAN_POINT('Ctrl Pts',(1.8489811319852,1.,-0.173946627587732));
#34191=CARTESIAN_POINT('Ctrl Pts',(1.83658380527692,1.,-0.1728894428919));
#34192=CARTESIAN_POINT('Ctrl Pts',(1.82215766811545,1.,-0.171554770204119));
#34193=CARTESIAN_POINT('Ctrl Pts',(1.80561530629706,1.,-0.169936923904608));
#34194=CARTESIAN_POINT('Ctrl Pts',(1.7869064998507,1.,-0.168032772805197));
#34195=CARTESIAN_POINT('Ctrl Pts',(1.77018771684844,1.,-0.1662793551464));
#34196=CARTESIAN_POINT('Ctrl Pts',(1.75666056638427,1.,-0.164834765707159));
#34197=CARTESIAN_POINT('Ctrl Pts',(1.7472034950333,1.,-0.163814161002002));
#34198=CARTESIAN_POINT('Ctrl Pts',(1.74236521665491,1.,-0.163289472382896));
#34199=CARTESIAN_POINT('',(2.19890268624765,0.,-0.0694764450219582));
#34200=CARTESIAN_POINT('Origin',(2.19890268624765,0.,0.0694764450219582));
#34201=CARTESIAN_POINT('',(2.19890268624765,1.,0.0694764450219582));
#34202=CARTESIAN_POINT('',(2.19890268624765,1.,-0.0694764450219582));
#34203=CARTESIAN_POINT('',(2.19890268624765,0.,0.0694764450219582));
#34204=CARTESIAN_POINT('Ctrl Pts',(1.74236521665491,-1.,0.163289472382896));
#34205=CARTESIAN_POINT('Ctrl Pts',(1.74236521665491,1.,0.163289472382896));
#34206=CARTESIAN_POINT('Ctrl Pts',(1.74720349503904,-1.,0.163814161002474));
#34207=CARTESIAN_POINT('Ctrl Pts',(1.74720349503904,1.,0.163814161002474));
#34208=CARTESIAN_POINT('Ctrl Pts',(1.75666056640041,-1.,0.164834765708484));
#34209=CARTESIAN_POINT('Ctrl Pts',(1.75666056640041,1.,0.164834765708484));
#34210=CARTESIAN_POINT('Ctrl Pts',(1.77018771687692,-1.,0.166279355148738));
#34211=CARTESIAN_POINT('Ctrl Pts',(1.77018771687692,1.,0.166279355148738));
#34212=CARTESIAN_POINT('Ctrl Pts',(1.78690649988931,-1.,0.16803277280837));
#34213=CARTESIAN_POINT('Ctrl Pts',(1.78690649988931,1.,0.16803277280837));
#34214=CARTESIAN_POINT('Ctrl Pts',(1.80561530633924,-1.,0.169936923908078));
#34215=CARTESIAN_POINT('Ctrl Pts',(1.80561530633924,1.,0.169936923908078));
#34216=CARTESIAN_POINT('Ctrl Pts',(1.82215766815414,-1.,0.171554770207306));
#34217=CARTESIAN_POINT('Ctrl Pts',(1.82215766815414,1.,0.171554770207306));
#34218=CARTESIAN_POINT('Ctrl Pts',(1.83658380530747,-1.,0.17288944289442));
#34219=CARTESIAN_POINT('Ctrl Pts',(1.83658380530747,1.,0.17288944289442));
#34220=CARTESIAN_POINT('Ctrl Pts',(1.84898113200543,-1.,0.173946627589401));
#34221=CARTESIAN_POINT('Ctrl Pts',(1.84898113200543,1.,0.173946627589401));
#34222=CARTESIAN_POINT('Ctrl Pts',(1.85948367089838,-1.,0.174735259276856));
#34223=CARTESIAN_POINT('Ctrl Pts',(1.85948367089838,1.,0.174735259276856));
#34224=CARTESIAN_POINT('Ctrl Pts',(1.86828349694972,-1.,0.1752683375909));
#34225=CARTESIAN_POINT('Ctrl Pts',(1.86828349694972,1.,0.1752683375909));
#34226=CARTESIAN_POINT('Ctrl Pts',(1.87563767773249,-1.,0.175563480746205));
#34227=CARTESIAN_POINT('Ctrl Pts',(1.87563767773249,1.,0.175563480746205));
#34228=CARTESIAN_POINT('Ctrl Pts',(1.88188663144846,-1.,0.175644148889271));
#34229=CARTESIAN_POINT('Ctrl Pts',(1.88188663144846,1.,0.175644148889271));
#34230=CARTESIAN_POINT('Ctrl Pts',(1.88742606272818,-1.,0.175538155840286));
#34231=CARTESIAN_POINT('Ctrl Pts',(1.88742606272818,1.,0.175538155840286));
#34232=CARTESIAN_POINT('Ctrl Pts',(1.89264630198279,-1.,0.175274276190664));
#34233=CARTESIAN_POINT('Ctrl Pts',(1.89264630198279,1.,0.175274276190664));
#34234=CARTESIAN_POINT('Ctrl Pts',(1.89788101117148,-1.,0.174879405091277));
#34235=CARTESIAN_POINT('Ctrl Pts',(1.89788101117148,1.,0.174879405091277));
#34236=CARTESIAN_POINT('Ctrl Pts',(1.90335253863003,-1.,0.174375518661222));
#34237=CARTESIAN_POINT('Ctrl Pts',(1.90335253863003,1.,0.174375518661222));
#34238=CARTESIAN_POINT('Ctrl Pts',(1.90911693975475,-1.,0.173776635257983));
#34239=CARTESIAN_POINT('Ctrl Pts',(1.90911693975475,1.,0.173776635257983));
#34240=CARTESIAN_POINT('Ctrl Pts',(1.91511429159681,-1.,0.173090695383619));
#34241=CARTESIAN_POINT('Ctrl Pts',(1.91511429159681,1.,0.173090695383619));
#34242=CARTESIAN_POINT('Ctrl Pts',(1.92122334398034,-1.,0.172321621259556));
#34243=CARTESIAN_POINT('Ctrl Pts',(1.92122334398034,1.,0.172321621259556));
#34244=CARTESIAN_POINT('Ctrl Pts',(1.92731093582,-1.,0.17147119153296));
#34245=CARTESIAN_POINT('Ctrl Pts',(1.92731093582,1.,0.17147119153296));
#34246=CARTESIAN_POINT('Ctrl Pts',(1.93329183155455,-1.,0.170541253116136));
#34247=CARTESIAN_POINT('Ctrl Pts',(1.93329183155455,1.,0.170541253116136));
#34248=CARTESIAN_POINT('Ctrl Pts',(1.93915639211497,-1.,0.169534904817425));
#34249=CARTESIAN_POINT('Ctrl Pts',(1.93915639211497,1.,0.169534904817425));
#34250=CARTESIAN_POINT('Ctrl Pts',(1.94493757756879,-1.,0.168455741607515));
#34251=CARTESIAN_POINT('Ctrl Pts',(1.94493757756879,1.,0.168455741607515));
#34252=CARTESIAN_POINT('Ctrl Pts',(1.95069027794286,-1.,0.167307501784469));
#34253=CARTESIAN_POINT('Ctrl Pts',(1.95069027794286,1.,0.167307501784469));
#34254=CARTESIAN_POINT('Ctrl Pts',(1.95646759718755,-1.,0.166093592002832));
#34255=CARTESIAN_POINT('Ctrl Pts',(1.95646759718755,1.,0.166093592002832));
#34256=CARTESIAN_POINT('Ctrl Pts',(1.96229379940174,-1.,0.1648165689203));
#34257=CARTESIAN_POINT('Ctrl Pts',(1.96229379940174,1.,0.1648165689203));
#34258=CARTESIAN_POINT('Ctrl Pts',(1.96816512678,-1.,0.16347818545776));
#34259=CARTESIAN_POINT('Ctrl Pts',(1.96816512678,1.,0.16347818545776));
#34260=CARTESIAN_POINT('Ctrl Pts',(1.97406280235204,-1.,0.162079693556302));
#34261=CARTESIAN_POINT('Ctrl Pts',(1.97406280235204,1.,0.162079693556302));
#34262=CARTESIAN_POINT('Ctrl Pts',(1.97996195437557,-1.,0.16062206078461));
#34263=CARTESIAN_POINT('Ctrl Pts',(1.97996195437557,1.,0.16062206078461));
#34264=CARTESIAN_POINT('Ctrl Pts',(1.98584238283279,-1.,0.159106226437288));
#34265=CARTESIAN_POINT('Ctrl Pts',(1.98584238283279,1.,0.159106226437288));
#34266=CARTESIAN_POINT('Ctrl Pts',(1.99169810931893,-1.,0.157533331459215));
#34267=CARTESIAN_POINT('Ctrl Pts',(1.99169810931893,1.,0.157533331459215));
#34268=CARTESIAN_POINT('Ctrl Pts',(1.99753284771487,-1.,0.155904629548774));
#34269=CARTESIAN_POINT('Ctrl Pts',(1.99753284771487,1.,0.155904629548774));
#34270=CARTESIAN_POINT('Ctrl Pts',(2.00335565310539,-1.,0.154221403049719));
#34271=CARTESIAN_POINT('Ctrl Pts',(2.00335565310539,1.,0.154221403049719));
#34272=CARTESIAN_POINT('Ctrl Pts',(2.00917680318426,-1.,0.152484883621452));
#34273=CARTESIAN_POINT('Ctrl Pts',(2.00917680318426,1.,0.152484883621452));
#34274=CARTESIAN_POINT('Ctrl Pts',(2.01500291940243,-1.,0.150696157673084));
#34275=CARTESIAN_POINT('Ctrl Pts',(2.01500291940243,1.,0.150696157673084));
#34276=CARTESIAN_POINT('Ctrl Pts',(2.02083464969897,-1.,0.148856124775342));
#34277=CARTESIAN_POINT('Ctrl Pts',(2.02083464969897,1.,0.148856124775342));
#34278=CARTESIAN_POINT('Ctrl Pts',(2.02666926182017,-1.,0.146965557332586));
#34279=CARTESIAN_POINT('Ctrl Pts',(2.02666926182017,1.,0.146965557332586));
#34280=CARTESIAN_POINT('Ctrl Pts',(2.03250223739941,-1.,0.145025140186058));
#34281=CARTESIAN_POINT('Ctrl Pts',(2.03250223739941,1.,0.145025140186058));
#34282=CARTESIAN_POINT('Ctrl Pts',(2.03832911025913,-1.,0.143035515058208));
#34283=CARTESIAN_POINT('Ctrl Pts',(2.03832911025913,1.,0.143035515058208));
#34284=CARTESIAN_POINT('Ctrl Pts',(2.04414757947919,-1.,0.140997332152545));
#34285=CARTESIAN_POINT('Ctrl Pts',(2.04414757947919,1.,0.140997332152545));
#34286=CARTESIAN_POINT('Ctrl Pts',(2.04995762001333,-1.,0.138911255368966));
#34287=CARTESIAN_POINT('Ctrl Pts',(2.04995762001333,1.,0.138911255368966));
#34288=CARTESIAN_POINT('Ctrl Pts',(2.0557604441427,-1.,0.136777941218044));
#34289=CARTESIAN_POINT('Ctrl Pts',(2.0557604441427,1.,0.136777941218044));
#34290=CARTESIAN_POINT('Ctrl Pts',(2.06155781517844,-1.,0.134598026192107));
#34291=CARTESIAN_POINT('Ctrl Pts',(2.06155781517844,1.,0.134598026192107));
#34292=CARTESIAN_POINT('Ctrl Pts',(2.06735123910319,-1.,0.132372111547709));
#34293=CARTESIAN_POINT('Ctrl Pts',(2.06735123910319,1.,0.132372111547709));
#34294=CARTESIAN_POINT('Ctrl Pts',(2.07314114713047,-1.,0.1301007483284));
#34295=CARTESIAN_POINT('Ctrl Pts',(2.07314114713047,1.,0.1301007483284));
#34296=CARTESIAN_POINT('Ctrl Pts',(2.07892715110967,-1.,0.127784445276116));
#34297=CARTESIAN_POINT('Ctrl Pts',(2.07892715110967,1.,0.127784445276116));
#34298=CARTESIAN_POINT('Ctrl Pts',(2.08470840653628,-1.,0.125423679412058));
#34299=CARTESIAN_POINT('Ctrl Pts',(2.08470840653628,1.,0.125423679412058));
#34300=CARTESIAN_POINT('Ctrl Pts',(2.09048392424826,-1.,0.123018905621083));
#34301=CARTESIAN_POINT('Ctrl Pts',(2.09048392424826,1.,0.123018905621083));
#34302=CARTESIAN_POINT('Ctrl Pts',(2.09625292867756,-1.,0.120570567965129));
#34303=CARTESIAN_POINT('Ctrl Pts',(2.09625292867756,1.,0.120570567965129));
#34304=CARTESIAN_POINT('Ctrl Pts',(2.10201512132945,-1.,0.118079107988368));
#34305=CARTESIAN_POINT('Ctrl Pts',(2.10201512132945,1.,0.118079107988368));
#34306=CARTESIAN_POINT('Ctrl Pts',(2.10777050261359,-1.,0.11554495768794));
#34307=CARTESIAN_POINT('Ctrl Pts',(2.10777050261359,1.,0.11554495768794));
#34308=CARTESIAN_POINT('Ctrl Pts',(2.11351924490335,-1.,0.112968534419746));
#34309=CARTESIAN_POINT('Ctrl Pts',(2.11351924490335,1.,0.112968534419746));
#34310=CARTESIAN_POINT('Ctrl Pts',(2.11926155590849,-1.,0.11035023613502));
#34311=CARTESIAN_POINT('Ctrl Pts',(2.11926155590849,1.,0.11035023613502));
#34312=CARTESIAN_POINT('Ctrl Pts',(2.12499752306927,-1.,0.107690435231068));
#34313=CARTESIAN_POINT('Ctrl Pts',(2.12499752306927,1.,0.107690435231068));
#34314=CARTESIAN_POINT('Ctrl Pts',(2.1307270488718,-1.,0.104989479152703));
#34315=CARTESIAN_POINT('Ctrl Pts',(2.1307270488718,1.,0.104989479152703));
#34316=CARTESIAN_POINT('Ctrl Pts',(2.13644992667052,-1.,0.102247700556063));
#34317=CARTESIAN_POINT('Ctrl Pts',(2.13644992667052,1.,0.102247700556063));
#34318=CARTESIAN_POINT('Ctrl Pts',(2.14216588395974,-1.,0.0994654261990741));
#34319=CARTESIAN_POINT('Ctrl Pts',(2.14216588395974,1.,0.0994654261990741));
#34320=CARTESIAN_POINT('Ctrl Pts',(2.14787463531864,-1.,0.0966429852305688));
#34321=CARTESIAN_POINT('Ctrl Pts',(2.14787463531864,1.,0.0966429852305688));
#34322=CARTESIAN_POINT('Ctrl Pts',(2.15357593978377,-1.,0.0937807218868344));
#34323=CARTESIAN_POINT('Ctrl Pts',(2.15357593978377,1.,0.0937807218868344));
#34324=CARTESIAN_POINT('Ctrl Pts',(2.15926961544808,-1.,0.0908789888108265));
#34325=CARTESIAN_POINT('Ctrl Pts',(2.15926961544808,1.,0.0908789888108265));
#34326=CARTESIAN_POINT('Ctrl Pts',(2.16495552645275,-1.,0.0879381291387821));
#34327=CARTESIAN_POINT('Ctrl Pts',(2.16495552645275,1.,0.0879381291387821));
#34328=CARTESIAN_POINT('Ctrl Pts',(2.17063357871031,-1.,0.0849584620835642));
#34329=CARTESIAN_POINT('Ctrl Pts',(2.17063357871031,1.,0.0849584620835642));
#34330=CARTESIAN_POINT('Ctrl Pts',(2.1763037121106,-1.,0.0819402680871938));
#34331=CARTESIAN_POINT('Ctrl Pts',(2.1763037121106,1.,0.0819402680871938));
#34332=CARTESIAN_POINT('Ctrl Pts',(2.18196589448304,-1.,0.0788837727683226));
#34333=CARTESIAN_POINT('Ctrl Pts',(2.18196589448304,1.,0.0788837727683226));
#34334=CARTESIAN_POINT('Ctrl Pts',(2.1876201139874,-1.,0.075789146583341));
#34335=CARTESIAN_POINT('Ctrl Pts',(2.1876201139874,1.,0.075789146583341));
#34336=CARTESIAN_POINT('Ctrl Pts',(2.19213712012956,-1.,0.0732830357304275));
#34337=CARTESIAN_POINT('Ctrl Pts',(2.19213712012956,1.,0.0732830357304275));
#34338=CARTESIAN_POINT('Ctrl Pts',(2.19552129483562,-1.,0.0713863779524626));
#34339=CARTESIAN_POINT('Ctrl Pts',(2.19552129483562,1.,0.0713863779524626));
#34340=CARTESIAN_POINT('Ctrl Pts',(2.19777582085261,-1.,0.0701143536324925));
#34341=CARTESIAN_POINT('Ctrl Pts',(2.19777582085261,1.,0.0701143536324925));
#34342=CARTESIAN_POINT('Ctrl Pts',(2.19890268624765,-1.,0.0694764450219582));
#34343=CARTESIAN_POINT('Ctrl Pts',(2.19890268624765,1.,0.0694764450219582));
#34344=CARTESIAN_POINT('',(1.74236521665491,1.,0.163289472382896));
#34345=CARTESIAN_POINT('Ctrl Pts',(1.74236521665491,1.,0.163289472382896));
#34346=CARTESIAN_POINT('Ctrl Pts',(1.74720349503904,1.,0.163814161002474));
#34347=CARTESIAN_POINT('Ctrl Pts',(1.75666056640041,1.,0.164834765708484));
#34348=CARTESIAN_POINT('Ctrl Pts',(1.77018771687692,1.,0.166279355148738));
#34349=CARTESIAN_POINT('Ctrl Pts',(1.78690649988931,1.,0.16803277280837));
#34350=CARTESIAN_POINT('Ctrl Pts',(1.80561530633924,1.,0.169936923908078));
#34351=CARTESIAN_POINT('Ctrl Pts',(1.82215766815414,1.,0.171554770207306));
#34352=CARTESIAN_POINT('Ctrl Pts',(1.83658380530747,1.,0.17288944289442));
#34353=CARTESIAN_POINT('Ctrl Pts',(1.84898113200543,1.,0.173946627589401));
#34354=CARTESIAN_POINT('Ctrl Pts',(1.85948367089838,1.,0.174735259276856));
#34355=CARTESIAN_POINT('Ctrl Pts',(1.86828349694972,1.,0.1752683375909));
#34356=CARTESIAN_POINT('Ctrl Pts',(1.87563767773249,1.,0.175563480746205));
#34357=CARTESIAN_POINT('Ctrl Pts',(1.88188663144846,1.,0.175644148889271));
#34358=CARTESIAN_POINT('Ctrl Pts',(1.88742606272818,1.,0.175538155840286));
#34359=CARTESIAN_POINT('Ctrl Pts',(1.89264630198279,1.,0.175274276190664));
#34360=CARTESIAN_POINT('Ctrl Pts',(1.89788101117148,1.,0.174879405091277));
#34361=CARTESIAN_POINT('Ctrl Pts',(1.90335253863003,1.,0.174375518661222));
#34362=CARTESIAN_POINT('Ctrl Pts',(1.90911693975475,1.,0.173776635257983));
#34363=CARTESIAN_POINT('Ctrl Pts',(1.91511429159681,1.,0.173090695383619));
#34364=CARTESIAN_POINT('Ctrl Pts',(1.92122334398034,1.,0.172321621259556));
#34365=CARTESIAN_POINT('Ctrl Pts',(1.92731093582,1.,0.17147119153296));
#34366=CARTESIAN_POINT('Ctrl Pts',(1.93329183155455,1.,0.170541253116136));
#34367=CARTESIAN_POINT('Ctrl Pts',(1.93915639211497,1.,0.169534904817425));
#34368=CARTESIAN_POINT('Ctrl Pts',(1.94493757756879,1.,0.168455741607515));
#34369=CARTESIAN_POINT('Ctrl Pts',(1.95069027794286,1.,0.167307501784469));
#34370=CARTESIAN_POINT('Ctrl Pts',(1.95646759718755,1.,0.166093592002832));
#34371=CARTESIAN_POINT('Ctrl Pts',(1.96229379940174,1.,0.1648165689203));
#34372=CARTESIAN_POINT('Ctrl Pts',(1.96816512678,1.,0.16347818545776));
#34373=CARTESIAN_POINT('Ctrl Pts',(1.97406280235204,1.,0.162079693556302));
#34374=CARTESIAN_POINT('Ctrl Pts',(1.97996195437557,1.,0.16062206078461));
#34375=CARTESIAN_POINT('Ctrl Pts',(1.98584238283279,1.,0.159106226437288));
#34376=CARTESIAN_POINT('Ctrl Pts',(1.99169810931893,1.,0.157533331459215));
#34377=CARTESIAN_POINT('Ctrl Pts',(1.99753284771487,1.,0.155904629548774));
#34378=CARTESIAN_POINT('Ctrl Pts',(2.00335565310539,1.,0.154221403049719));
#34379=CARTESIAN_POINT('Ctrl Pts',(2.00917680318426,1.,0.152484883621452));
#34380=CARTESIAN_POINT('Ctrl Pts',(2.01500291940243,1.,0.150696157673084));
#34381=CARTESIAN_POINT('Ctrl Pts',(2.02083464969897,1.,0.148856124775342));
#34382=CARTESIAN_POINT('Ctrl Pts',(2.02666926182017,1.,0.146965557332586));
#34383=CARTESIAN_POINT('Ctrl Pts',(2.03250223739941,1.,0.145025140186058));
#34384=CARTESIAN_POINT('Ctrl Pts',(2.03832911025913,1.,0.143035515058208));
#34385=CARTESIAN_POINT('Ctrl Pts',(2.04414757947919,1.,0.140997332152545));
#34386=CARTESIAN_POINT('Ctrl Pts',(2.04995762001333,1.,0.138911255368966));
#34387=CARTESIAN_POINT('Ctrl Pts',(2.0557604441427,1.,0.136777941218044));
#34388=CARTESIAN_POINT('Ctrl Pts',(2.06155781517844,1.,0.134598026192107));
#34389=CARTESIAN_POINT('Ctrl Pts',(2.06735123910319,1.,0.132372111547709));
#34390=CARTESIAN_POINT('Ctrl Pts',(2.07314114713047,1.,0.1301007483284));
#34391=CARTESIAN_POINT('Ctrl Pts',(2.07892715110967,1.,0.127784445276116));
#34392=CARTESIAN_POINT('Ctrl Pts',(2.08470840653628,1.,0.125423679412058));
#34393=CARTESIAN_POINT('Ctrl Pts',(2.09048392424826,1.,0.123018905621083));
#34394=CARTESIAN_POINT('Ctrl Pts',(2.09625292867756,1.,0.120570567965129));
#34395=CARTESIAN_POINT('Ctrl Pts',(2.10201512132945,1.,0.118079107988368));
#34396=CARTESIAN_POINT('Ctrl Pts',(2.10777050261359,1.,0.11554495768794));
#34397=CARTESIAN_POINT('Ctrl Pts',(2.11351924490335,1.,0.112968534419746));
#34398=CARTESIAN_POINT('Ctrl Pts',(2.11926155590849,1.,0.11035023613502));
#34399=CARTESIAN_POINT('Ctrl Pts',(2.12499752306927,1.,0.107690435231068));
#34400=CARTESIAN_POINT('Ctrl Pts',(2.1307270488718,1.,0.104989479152703));
#34401=CARTESIAN_POINT('Ctrl Pts',(2.13644992667052,1.,0.102247700556063));
#34402=CARTESIAN_POINT('Ctrl Pts',(2.14216588395974,1.,0.0994654261990741));
#34403=CARTESIAN_POINT('Ctrl Pts',(2.14787463531864,1.,0.0966429852305688));
#34404=CARTESIAN_POINT('Ctrl Pts',(2.15357593978377,1.,0.0937807218868344));
#34405=CARTESIAN_POINT('Ctrl Pts',(2.15926961544808,1.,0.0908789888108265));
#34406=CARTESIAN_POINT('Ctrl Pts',(2.16495552645275,1.,0.0879381291387821));
#34407=CARTESIAN_POINT('Ctrl Pts',(2.17063357871031,1.,0.0849584620835642));
#34408=CARTESIAN_POINT('Ctrl Pts',(2.1763037121106,1.,0.0819402680871938));
#34409=CARTESIAN_POINT('Ctrl Pts',(2.18196589448304,1.,0.0788837727683226));
#34410=CARTESIAN_POINT('Ctrl Pts',(2.1876201139874,1.,0.075789146583341));
#34411=CARTESIAN_POINT('Ctrl Pts',(2.19213712012956,1.,0.0732830357304275));
#34412=CARTESIAN_POINT('Ctrl Pts',(2.19552129483562,1.,0.0713863779524626));
#34413=CARTESIAN_POINT('Ctrl Pts',(2.19777582085261,1.,0.0701143536324925));
#34414=CARTESIAN_POINT('Ctrl Pts',(2.19890268624765,1.,0.0694764450219582));
#34415=CARTESIAN_POINT('',(1.74236521665491,0.,0.163289472382896));
#34416=CARTESIAN_POINT('Origin',(0.,1.,0.));
#34417=CARTESIAN_POINT('Origin',(0.,1.,0.));
#34418=CARTESIAN_POINT('Origin',(0.,0.,0.));
#34419=CARTESIAN_POINT('',(0.,0.,0.));
#34420=CARTESIAN_POINT('Origin',(0.3,0.4,0.));
#34421=CARTESIAN_POINT('',(-0.3,0.4,-3.67394039744206E-17));
#34422=CARTESIAN_POINT('Origin',(0.,0.4,0.));
#34423=CARTESIAN_POINT('Origin',(0.,0.375,0.));
#34424=CARTESIAN_POINT('',(-0.35,0.35,-4.28626379701573E-17));
#34425=CARTESIAN_POINT('Origin',(0.,0.35,0.));
#34426=CARTESIAN_POINT('',(-0.325,0.375,-3.9801020972289E-17));
#34427=CARTESIAN_POINT('Origin',(0.,0.19,0.));
#34428=CARTESIAN_POINT('',(-0.35,0.03,-4.28626379701574E-17));
#34429=CARTESIAN_POINT('Origin',(0.,0.03,0.));
#34430=CARTESIAN_POINT('',(-0.35,0.19,-4.28626379701574E-17));
#34431=CARTESIAN_POINT('Origin',(0.,0.0149999999999999,0.));
#34432=CARTESIAN_POINT('',(-0.32,-3.29597460435593E-17,-3.91886975727153E-17));
#34433=CARTESIAN_POINT('Origin',(0.,0.,0.));
#34434=CARTESIAN_POINT('',(-0.335,0.0149999999999999,-4.10256677714363E-17));
#34435=CARTESIAN_POINT('Origin',(0.22,0.,0.));
#34436=CARTESIAN_POINT('',(-0.22,-6.93889390390723E-18,-2.69422295812418E-17));
#34437=CARTESIAN_POINT('Origin',(0.,0.,0.));
#34438=CARTESIAN_POINT('Origin',(0.,-0.02,0.));
#34439=CARTESIAN_POINT('',(-0.1954,-0.0492,2.39295984553393E-17));
#34440=CARTESIAN_POINT('Origin',(0.,-0.0492,0.));
#34441=CARTESIAN_POINT('',(-0.21,-0.02,-2.57175827820944E-17));
#34442=CARTESIAN_POINT('Origin',(0.,-0.8,0.));
#34443=CARTESIAN_POINT('',(-0.1954,-1.5646,2.39295984553393E-17));
#34444=CARTESIAN_POINT('Origin',(0.,-1.5646,0.));
#34445=CARTESIAN_POINT('',(-0.1954,-0.8,-2.39295984553393E-17));
#34446=CARTESIAN_POINT('Origin',(0.,-1.58,0.));
#34447=CARTESIAN_POINT('',(-0.16,-1.6,-1.95943487863577E-17));
#34448=CARTESIAN_POINT('Origin',(0.,-1.6,0.));
#34449=CARTESIAN_POINT('',(-0.18,-1.58,-2.20436423846524E-17));
#34450=CARTESIAN_POINT('Origin',(0.,-1.6,0.));
#34451=CARTESIAN_POINT('Origin',(0.0866025403784439,-0.4,-0.15));
#34452=CARTESIAN_POINT('',(0.173205080756888,-0.4,0.));
#34453=CARTESIAN_POINT('',(0.0866025403784439,-0.4,-0.15));
#34454=CARTESIAN_POINT('',(0.173205080756888,-0.4,0.));
#34455=CARTESIAN_POINT('',(0.0866025403784439,-0.64,-0.15));
#34456=CARTESIAN_POINT('',(0.0866025403784439,-0.4,-0.15));
#34457=CARTESIAN_POINT('',(0.173205080756888,-0.64,0.));
#34458=CARTESIAN_POINT('',(0.173205080756888,-0.64,0.));
#34459=CARTESIAN_POINT('',(0.173205080756888,-0.4,0.));
#34460=CARTESIAN_POINT('Origin',(-0.0866025403784438,-0.4,-0.15));
#34461=CARTESIAN_POINT('',(-0.0866025403784438,-0.4,-0.15));
#34462=CARTESIAN_POINT('',(0.0866025403784439,-0.4,-0.15));
#34463=CARTESIAN_POINT('',(-0.0866025403784438,-0.64,-0.15));
#34464=CARTESIAN_POINT('',(-0.0866025403784438,-0.4,-0.15));
#34465=CARTESIAN_POINT('',(0.0866025403784439,-0.64,-0.15));
#34466=CARTESIAN_POINT('Origin',(-0.173205080756888,-0.4,-2.77555756156289E-17));
#34467=CARTESIAN_POINT('',(-0.173205080756888,-0.4,-2.12115047744981E-17));
#34468=CARTESIAN_POINT('',(-0.0866025403784438,-0.4,-0.15));
#34469=CARTESIAN_POINT('',(-0.173205080756888,-0.64,-2.77555756156289E-17));
#34470=CARTESIAN_POINT('',(-0.173205080756888,-0.4,-2.12115047744981E-17));
#34471=CARTESIAN_POINT('',(-0.0866025403784438,-0.64,-0.15));
#34472=CARTESIAN_POINT('Origin',(-0.0866025403784439,-0.4,0.15));
#34473=CARTESIAN_POINT('',(-0.0866025403784439,-0.4,0.15));
#34474=CARTESIAN_POINT('',(-0.173205080756888,-0.4,-2.12115047744981E-17));
#34475=CARTESIAN_POINT('',(-0.0866025403784439,-0.64,0.15));
#34476=CARTESIAN_POINT('',(-0.0866025403784439,-0.4,0.15));
#34477=CARTESIAN_POINT('',(-0.173205080756888,-0.64,-2.12115047744981E-17));
#34478=CARTESIAN_POINT('Origin',(0.0866025403784439,-0.4,0.15));
#34479=CARTESIAN_POINT('',(0.0866025403784439,-0.4,0.15));
#34480=CARTESIAN_POINT('',(-0.0866025403784439,-0.4,0.15));
#34481=CARTESIAN_POINT('',(0.0866025403784439,-0.64,0.15));
#34482=CARTESIAN_POINT('',(0.0866025403784439,-0.4,0.15));
#34483=CARTESIAN_POINT('',(-0.0866025403784439,-0.64,0.15));
#34484=CARTESIAN_POINT('Origin',(0.173205080756888,-0.4,0.));
#34485=CARTESIAN_POINT('',(0.0866025403784439,-0.4,0.15));
#34486=CARTESIAN_POINT('',(0.0866025403784439,-0.64,0.15));
#34487=CARTESIAN_POINT('Origin',(0.,-0.4,-2.77555756156289E-17));
#34488=CARTESIAN_POINT('Origin',(0.,-0.64,-2.77555756156289E-17));
#34489=CARTESIAN_POINT('',(0.,0.,0.));
#34490=CARTESIAN_POINT('',(0.,0.,0.));
#34491=CARTESIAN_POINT('',(0.,0.,0.));
#34492=CARTESIAN_POINT('',(0.,0.,0.));
#34493=CARTESIAN_POINT('',(0.,0.,0.));
#34494=CARTESIAN_POINT('',(0.,0.,0.));
#34495=CARTESIAN_POINT('',(0.,0.,0.));
#34496=CARTESIAN_POINT('',(0.,0.,0.));
#34497=CARTESIAN_POINT('',(0.,0.,0.));
#34498=CARTESIAN_POINT('',(0.,0.,0.));
#34499=CARTESIAN_POINT('',(0.,0.,0.));
#34500=CARTESIAN_POINT('',(0.,0.,0.));
#34501=CARTESIAN_POINT('',(0.,0.,0.));
#34502=CARTESIAN_POINT('',(0.,0.,0.));
#34503=CARTESIAN_POINT('',(1.,-4.,2.));
#34504=CARTESIAN_POINT('',(1.,4.,2.));
#34505=CARTESIAN_POINT('',(2.5,-4.,2.42));
#34506=CARTESIAN_POINT('',(2.5,-4.,3.8));
#34507=CARTESIAN_POINT('',(2.5,-4.,3.9));
#34508=CARTESIAN_POINT('',(2.5,-4.,1.58));
#34509=CARTESIAN_POINT('',(2.5,-4.,0.));
#34510=CARTESIAN_POINT('',(2.5,-4.,-0.1));
#34511=CARTESIAN_POINT('',(2.5,4.,2.42));
#34512=CARTESIAN_POINT('',(2.5,4.,3.8));
#34513=CARTESIAN_POINT('',(2.5,4.,3.9));
#34514=CARTESIAN_POINT('',(2.5,4.,1.58));
#34515=CARTESIAN_POINT('',(2.5,4.,0.));
#34516=CARTESIAN_POINT('',(2.5,4.,-0.1));
#34517=CARTESIAN_POINT('',(19.5,-4.,2.42));
#34518=CARTESIAN_POINT('',(19.5,-4.,3.8));
#34519=CARTESIAN_POINT('',(19.5,-4.,3.9));
#34520=CARTESIAN_POINT('',(19.5,-4.,1.58));
#34521=CARTESIAN_POINT('',(19.5,-4.,0.));
#34522=CARTESIAN_POINT('',(19.5,-4.,-0.1));
#34523=CARTESIAN_POINT('',(19.5,4.,2.42));
#34524=CARTESIAN_POINT('',(19.5,4.,3.8));
#34525=CARTESIAN_POINT('',(19.5,4.,3.9));
#34526=CARTESIAN_POINT('',(19.5,4.,1.58));
#34527=CARTESIAN_POINT('',(19.5,4.,0.));
#34528=CARTESIAN_POINT('',(19.5,4.,-0.1));
#34529=CARTESIAN_POINT('',(0.,0.,3.8));
#34530=CARTESIAN_POINT('',(2.,0.,4.77));
#34531=CARTESIAN_POINT('',(8.,0.,4.77));
#34532=CARTESIAN_POINT('',(14.,0.,4.77));
#34533=CARTESIAN_POINT('',(20.,0.,4.77));
#34534=CARTESIAN_POINT('',(-4.2,-1.8,4.8));
#34535=CARTESIAN_POINT('',(-4.2,1.8,4.8));
#34536=CARTESIAN_POINT('',(26.2,-1.8,4.8));
#34537=CARTESIAN_POINT('',(26.2,1.8,4.8));
#34538=CARTESIAN_POINT('',(8.,-4.2,4.6));
#34539=CARTESIAN_POINT('',(14.,-4.2,4.6));
#34540=CARTESIAN_POINT('',(11.,-4.2,10.25));
#34541=CARTESIAN_POINT('',(12.4849242404918,-5.2,11.7349242404918));
#34542=CARTESIAN_POINT('',(9.51507575950825,-5.2,11.7349242404918));
#34543=CARTESIAN_POINT('',(9.51507575950825,-5.2,8.76507575950825));
#34544=CARTESIAN_POINT('',(12.4849242404917,-5.2,8.76507575950825));
#34545=CARTESIAN_POINT('',(12.4849242404918,-3.2,11.7349242404918));
#34546=CARTESIAN_POINT('',(9.51507575950825,-3.2,11.7349242404918));
#34547=CARTESIAN_POINT('',(9.51507575950825,-3.2,8.76507575950825));
#34548=CARTESIAN_POINT('',(12.4849242404917,-3.2,8.76507575950825));
#34549=CARTESIAN_POINT('',(8.,4.2,4.6));
#34550=CARTESIAN_POINT('',(14.,4.2,4.6));
#34551=CARTESIAN_POINT('',(11.,4.2,10.25));
#34552=CARTESIAN_POINT('',(12.4849242404918,3.2,11.7349242404918));
#34553=CARTESIAN_POINT('',(9.51507575950825,3.2,11.7349242404918));
#34554=CARTESIAN_POINT('',(9.51507575950825,3.2,8.76507575950825));
#34555=CARTESIAN_POINT('',(12.4849242404918,3.2,8.76507575950825));
#34556=CARTESIAN_POINT('',(12.4849242404918,5.2,11.7349242404918));
#34557=CARTESIAN_POINT('',(9.51507575950825,5.2,11.7349242404918));
#34558=CARTESIAN_POINT('',(9.51507575950825,5.2,8.76507575950825));
#34559=CARTESIAN_POINT('',(12.4849242404918,5.2,8.76507575950825));
#34560=CARTESIAN_POINT('',(0.,0.,0.));
#34561=CARTESIAN_POINT('',(0.,0.,0.));
#34562=CARTESIAN_POINT('',(11.,0.,3.8));
#34563=CARTESIAN_POINT('',(9.5,-1.9,7.));
#34564=CARTESIAN_POINT('',(9.5,1.9,7.));
#34565=CARTESIAN_POINT('',(12.5,-1.9,7.));
#34566=CARTESIAN_POINT('',(12.5,1.9,7.));
#34567=CARTESIAN_POINT('',(5.,-0.6,6.2));
#34568=CARTESIAN_POINT('',(5.,0.6,6.2));
#34569=CARTESIAN_POINT('',(17.,-0.6,6.2));
#34570=CARTESIAN_POINT('',(17.,0.6,6.2));
#34571=CARTESIAN_POINT('',(0.,0.,0.));
#34572=CARTESIAN_POINT('Origin',(0.7,0.,0.25));
#34573=CARTESIAN_POINT('',(0.7,0.16,0.4));
#34574=CARTESIAN_POINT('',(0.7,0.2,0.36));
#34575=CARTESIAN_POINT('',(0.7,0.1675,0.3925));
#34576=CARTESIAN_POINT('',(0.7,-0.16,0.4));
#34577=CARTESIAN_POINT('',(0.7,0.,0.4));
#34578=CARTESIAN_POINT('',(0.7,-0.2,0.36));
#34579=CARTESIAN_POINT('',(0.7,-0.1675,0.3925));
#34580=CARTESIAN_POINT('',(0.7,-0.2,0.04));
#34581=CARTESIAN_POINT('',(0.7,-0.2,0.125));
#34582=CARTESIAN_POINT('',(0.7,-0.16,0.));
#34583=CARTESIAN_POINT('',(0.7,-0.1925,0.0325));
#34584=CARTESIAN_POINT('',(0.7,0.16,0.));
#34585=CARTESIAN_POINT('',(0.7,0.,0.));
#34586=CARTESIAN_POINT('',(0.7,0.2,0.04));
#34587=CARTESIAN_POINT('',(0.7,0.1925,0.0325));
#34588=CARTESIAN_POINT('',(0.7,0.2,0.125));
#34589=CARTESIAN_POINT('Origin',(-0.4,-0.18,0.02));
#34590=CARTESIAN_POINT('',(-0.7,-0.2,0.04));
#34591=CARTESIAN_POINT('',(-0.4,-0.2,0.04));
#34592=CARTESIAN_POINT('',(-0.7,-0.16,0.));
#34593=CARTESIAN_POINT('',(-0.7,-0.1925,0.0325));
#34594=CARTESIAN_POINT('',(-0.4,-0.16,0.));
#34595=CARTESIAN_POINT('Origin',(-0.8,-0.2,0.));
#34596=CARTESIAN_POINT('',(-0.7,-0.2,0.36));
#34597=CARTESIAN_POINT('',(-0.4,-0.2,0.36));
#34598=CARTESIAN_POINT('',(-0.7,-0.2,0.125));
#34599=CARTESIAN_POINT('Origin',(-0.4,-0.18,0.38));
#34600=CARTESIAN_POINT('',(-0.7,-0.16,0.4));
#34601=CARTESIAN_POINT('',(-0.4,-0.16,0.4));
#34602=CARTESIAN_POINT('',(-0.7,-0.1675,0.3925));
#34603=CARTESIAN_POINT('Origin',(0.,0.,0.4));
#34604=CARTESIAN_POINT('',(-0.7,0.16,0.4));
#34605=CARTESIAN_POINT('',(0.4,0.16,0.4));
#34606=CARTESIAN_POINT('',(-0.7,0.,0.4));
#34607=CARTESIAN_POINT('Origin',(-0.7,0.,0.25));
#34608=CARTESIAN_POINT('',(-0.7,0.2,0.36));
#34609=CARTESIAN_POINT('',(-0.7,0.1675,0.3925));
#34610=CARTESIAN_POINT('',(-0.7,0.2,0.04));
#34611=CARTESIAN_POINT('',(-0.7,0.2,0.125));
#34612=CARTESIAN_POINT('',(-0.7,0.16,0.));
#34613=CARTESIAN_POINT('',(-0.7,0.1925,0.0325));
#34614=CARTESIAN_POINT('',(-0.7,0.,0.));
#34615=CARTESIAN_POINT('Origin',(0.4,0.18,0.38));
#34616=CARTESIAN_POINT('',(0.4,0.2,0.36));
#34617=CARTESIAN_POINT('Origin',(0.8,0.2,0.));
#34618=CARTESIAN_POINT('',(0.4,0.2,0.04));
#34619=CARTESIAN_POINT('Origin',(0.4,0.18,0.02));
#34620=CARTESIAN_POINT('',(0.4,0.16,0.));
#34621=CARTESIAN_POINT('Origin',(0.,0.,0.));
#34622=CARTESIAN_POINT('',(0.,0.,0.));
#34623=CARTESIAN_POINT('Origin',(0.,0.,0.));
#34624=CARTESIAN_POINT('',(-0.32,0.16,3.91886975727153E-17));
#34625=CARTESIAN_POINT('Origin',(0.,0.16,0.));
#34626=CARTESIAN_POINT('',(-0.32,0.,3.91886975727153E-17));
#34627=CARTESIAN_POINT('',(-0.32,0.,3.91886975727153E-17));
#34628=CARTESIAN_POINT('Origin',(0.,0.,0.));
#34629=CARTESIAN_POINT('Origin',(0.,0.,0.));
#34630=CARTESIAN_POINT('',(-0.6,0.16,7.34788079488412E-17));
#34631=CARTESIAN_POINT('Origin',(0.,0.16,0.));
#34632=CARTESIAN_POINT('',(-0.6,0.,7.34788079488412E-17));
#34633=CARTESIAN_POINT('',(-0.6,0.,7.34788079488412E-17));
#34634=CARTESIAN_POINT('Origin',(0.,0.,0.));
#34635=CARTESIAN_POINT('Origin',(0.,0.16,0.));
#34636=CARTESIAN_POINT('Origin',(0.,0.,0.));
#34637=CARTESIAN_POINT('',(0.,0.,0.));
#34638=CARTESIAN_POINT('Origin',(0.45,0.6,0.));
#34639=CARTESIAN_POINT('',(-0.45,0.6,-5.51091059616309E-17));
#34640=CARTESIAN_POINT('Origin',(0.,0.6,0.));
#34641=CARTESIAN_POINT('Origin',(0.,0.575,0.));
#34642=CARTESIAN_POINT('',(-0.5,0.55,-6.12323399573677E-17));
#34643=CARTESIAN_POINT('Origin',(0.,0.55,0.));
#34644=CARTESIAN_POINT('',(-0.475,0.575,-5.81707229594993E-17));
#34645=CARTESIAN_POINT('Origin',(0.,0.29,0.));
#34646=CARTESIAN_POINT('',(-0.5,0.0299999999999998,-6.12323399573677E-17));
#34647=CARTESIAN_POINT('Origin',(0.,0.0299999999999998,0.));
#34648=CARTESIAN_POINT('',(-0.5,0.29,-6.12323399573677E-17));
#34649=CARTESIAN_POINT('Origin',(0.,0.0150000000000001,0.));
#34650=CARTESIAN_POINT('',(-0.47,7.11236625150491E-17,-5.75583995599256E-17));
#34651=CARTESIAN_POINT('Origin',(0.,0.,0.));
#34652=CARTESIAN_POINT('',(-0.485,0.0150000000000001,-5.93953697586466E-17));
#34653=CARTESIAN_POINT('Origin',(0.32,0.,0.));
#34654=CARTESIAN_POINT('',(-0.32,-6.93889390390723E-18,-3.91886975727153E-17));
#34655=CARTESIAN_POINT('Origin',(0.,0.,0.));
#34656=CARTESIAN_POINT('Origin',(0.,-0.02,0.));
#34657=CARTESIAN_POINT('',(-0.2942,-0.0515999999999999,3.60291088309151E-17));
#34658=CARTESIAN_POINT('Origin',(0.,-0.0515999999999999,0.));
#34659=CARTESIAN_POINT('',(-0.31,-0.02,-3.7964050773568E-17));
#34660=CARTESIAN_POINT('Origin',(0.,-1.24,0.));
#34661=CARTESIAN_POINT('',(-0.2942,-2.4458,3.60291088309151E-17));
#34662=CARTESIAN_POINT('Origin',(0.,-2.4458,0.));
#34663=CARTESIAN_POINT('',(-0.2942,-1.24,-3.60291088309151E-17));
#34664=CARTESIAN_POINT('Origin',(0.,-2.47,0.));
#34665=CARTESIAN_POINT('',(-0.24,-2.5,-2.93915231795365E-17));
#34666=CARTESIAN_POINT('Origin',(0.,-2.5,0.));
#34667=CARTESIAN_POINT('',(-0.27,-2.47,-3.30654635769785E-17));
#34668=CARTESIAN_POINT('Origin',(0.,-2.5,0.));
#34669=CARTESIAN_POINT('Origin',(0.144337567297406,-0.6,-0.25));
#34670=CARTESIAN_POINT('',(0.288675134594813,-0.6,0.));
#34671=CARTESIAN_POINT('',(0.144337567297406,-0.6,-0.25));
#34672=CARTESIAN_POINT('',(0.288675134594813,-0.6,0.));
#34673=CARTESIAN_POINT('',(0.144337567297406,-0.96,-0.25));
#34674=CARTESIAN_POINT('',(0.144337567297406,-0.6,-0.25));
#34675=CARTESIAN_POINT('',(0.288675134594813,-0.96,0.));
#34676=CARTESIAN_POINT('',(0.288675134594813,-0.96,0.));
#34677=CARTESIAN_POINT('',(0.288675134594813,-0.6,0.));
#34678=CARTESIAN_POINT('Origin',(-0.144337567297406,-0.6,-0.25));
#34679=CARTESIAN_POINT('',(-0.144337567297406,-0.6,-0.25));
#34680=CARTESIAN_POINT('',(0.144337567297406,-0.6,-0.25));
#34681=CARTESIAN_POINT('',(-0.144337567297406,-0.96,-0.25));
#34682=CARTESIAN_POINT('',(-0.144337567297406,-0.6,-0.25));
#34683=CARTESIAN_POINT('',(0.144337567297406,-0.96,-0.25));
#34684=CARTESIAN_POINT('Origin',(-0.288675134594813,-0.6,-8.32667268468867E-17));
#34685=CARTESIAN_POINT('',(-0.288675134594813,-0.6,-3.53525079574969E-17));
#34686=CARTESIAN_POINT('',(-0.144337567297406,-0.6,-0.25));
#34687=CARTESIAN_POINT('',(-0.288675134594813,-0.96,-5.55111512312578E-17));
#34688=CARTESIAN_POINT('',(-0.288675134594813,-0.6,-3.53525079574969E-17));
#34689=CARTESIAN_POINT('',(-0.144337567297406,-0.96,-0.25));
#34690=CARTESIAN_POINT('Origin',(-0.144337567297407,-0.6,0.25));
#34691=CARTESIAN_POINT('',(-0.144337567297407,-0.6,0.25));
#34692=CARTESIAN_POINT('',(-0.288675134594813,-0.6,-3.53525079574969E-17));
#34693=CARTESIAN_POINT('',(-0.144337567297407,-0.96,0.25));
#34694=CARTESIAN_POINT('',(-0.144337567297407,-0.6,0.25));
#34695=CARTESIAN_POINT('',(-0.288675134594813,-0.96,-3.53525079574969E-17));
#34696=CARTESIAN_POINT('Origin',(0.144337567297406,-0.6,0.25));
#34697=CARTESIAN_POINT('',(0.144337567297406,-0.6,0.25));
#34698=CARTESIAN_POINT('',(-0.144337567297407,-0.6,0.25));
#34699=CARTESIAN_POINT('',(0.144337567297406,-0.96,0.25));
#34700=CARTESIAN_POINT('',(0.144337567297406,-0.6,0.25));
#34701=CARTESIAN_POINT('',(-0.144337567297407,-0.96,0.25));
#34702=CARTESIAN_POINT('Origin',(0.288675134594813,-0.6,0.));
#34703=CARTESIAN_POINT('',(0.144337567297406,-0.6,0.25));
#34704=CARTESIAN_POINT('',(0.144337567297406,-0.96,0.25));
#34705=CARTESIAN_POINT('Origin',(0.,-0.6,0.));
#34706=CARTESIAN_POINT('Origin',(0.,-0.96,0.));
#34707=CARTESIAN_POINT('',(0.,0.,0.));
#34708=CARTESIAN_POINT('',(0.,0.,0.));
#34709=CARTESIAN_POINT('',(0.,0.,0.));
#34710=CARTESIAN_POINT('',(0.,0.,0.));
#34711=CARTESIAN_POINT('',(0.,0.,0.));
#34712=CARTESIAN_POINT('',(0.,0.,0.));
#34713=CARTESIAN_POINT('',(0.,0.,0.));
#34714=CARTESIAN_POINT('',(0.,0.,0.));
#34715=CARTESIAN_POINT('',(0.,0.,0.));
#34716=CARTESIAN_POINT('',(11.,0.,10.25));
#34717=CARTESIAN_POINT('',(11.,0.5,9.9));
#34718=CARTESIAN_POINT('',(11.,-6.7,10.25));
#34719=CARTESIAN_POINT('',(11.,8.1,10.25));
#34720=CARTESIAN_POINT('',(11.,6.9,9.9));
#34721=CARTESIAN_POINT('',(11.,8.9,13.25));
#34722=CARTESIAN_POINT('',(11.,9.06,13.25));
#34723=CARTESIAN_POINT('',(0.,0.,0.));
#34724=CARTESIAN_POINT('',(0.,0.,0.));
#34725=CARTESIAN_POINT('Origin',(11.,7.3,13.25));
#34726=CARTESIAN_POINT('',(10.595,8.87,13.25));
#34727=CARTESIAN_POINT('Origin',(11.,8.87,13.25));
#34728=CARTESIAN_POINT('',(10.595,7.3,13.25));
#34729=CARTESIAN_POINT('',(10.595,7.3,13.25));
#34730=CARTESIAN_POINT('Origin',(11.,7.3,13.25));
#34731=CARTESIAN_POINT('Origin',(11.,7.3,13.25));
#34732=CARTESIAN_POINT('',(10.1,8.87,13.25));
#34733=CARTESIAN_POINT('Origin',(11.,8.87,13.25));
#34734=CARTESIAN_POINT('',(10.1,7.3,13.25));
#34735=CARTESIAN_POINT('',(10.1,7.3,13.25));
#34736=CARTESIAN_POINT('Origin',(11.,7.3,13.25));
#34737=CARTESIAN_POINT('Origin',(11.,8.87,13.25));
#34738=CARTESIAN_POINT('Origin',(11.,7.3,13.25));
#34739=CARTESIAN_POINT('',(0.,0.,0.));
#34740=CARTESIAN_POINT('',(0.,0.,0.));
#34741=CARTESIAN_POINT('',(0.,0.,0.));
#34742=CARTESIAN_POINT('',(0.,0.,0.));
#34743=CARTESIAN_POINT('',(0.,0.,0.));
#34744=UNCERTAINTY_MEASURE_WITH_UNIT(LENGTH_MEASURE(0.001),#34852,
'DISTANCE_ACCURACY_VALUE',
'Maximum model space distance between geometric entities at asserted c
onnectivities');
#34745=UNCERTAINTY_MEASURE_WITH_UNIT(LENGTH_MEASURE(0.001),#34852,
'DISTANCE_ACCURACY_VALUE',
'Maximum model space distance between geometric entities at asserted c
onnectivities');
#34746=UNCERTAINTY_MEASURE_WITH_UNIT(LENGTH_MEASURE(0.001),#34852,
'DISTANCE_ACCURACY_VALUE',
'Maximum model space distance between geometric entities at asserted c
onnectivities');
#34747=UNCERTAINTY_MEASURE_WITH_UNIT(LENGTH_MEASURE(0.001),#34852,
'DISTANCE_ACCURACY_VALUE',
'Maximum model space distance between geometric entities at asserted c
onnectivities');
#34748=UNCERTAINTY_MEASURE_WITH_UNIT(LENGTH_MEASURE(0.001),#34852,
'DISTANCE_ACCURACY_VALUE',
'Maximum model space distance between geometric entities at asserted c
onnectivities');
#34749=UNCERTAINTY_MEASURE_WITH_UNIT(LENGTH_MEASURE(0.001),#34852,
'DISTANCE_ACCURACY_VALUE',
'Maximum model space distance between geometric entities at asserted c
onnectivities');
#34750=UNCERTAINTY_MEASURE_WITH_UNIT(LENGTH_MEASURE(0.001),#34852,
'DISTANCE_ACCURACY_VALUE',
'Maximum model space distance between geometric entities at asserted c
onnectivities');
#34751=UNCERTAINTY_MEASURE_WITH_UNIT(LENGTH_MEASURE(0.001),#34852,
'DISTANCE_ACCURACY_VALUE',
'Maximum model space distance between geometric entities at asserted c
onnectivities');
#34752=UNCERTAINTY_MEASURE_WITH_UNIT(LENGTH_MEASURE(0.001),#34852,
'DISTANCE_ACCURACY_VALUE',
'Maximum model space distance between geometric entities at asserted c
onnectivities');
#34753=UNCERTAINTY_MEASURE_WITH_UNIT(LENGTH_MEASURE(0.001),#34852,
'DISTANCE_ACCURACY_VALUE',
'Maximum model space distance between geometric entities at asserted c
onnectivities');
#34754=UNCERTAINTY_MEASURE_WITH_UNIT(LENGTH_MEASURE(0.001),#34852,
'DISTANCE_ACCURACY_VALUE',
'Maximum model space distance between geometric entities at asserted c
onnectivities');
#34755=UNCERTAINTY_MEASURE_WITH_UNIT(LENGTH_MEASURE(0.001),#34852,
'DISTANCE_ACCURACY_VALUE',
'Maximum model space distance between geometric entities at asserted c
onnectivities');
#34756=UNCERTAINTY_MEASURE_WITH_UNIT(LENGTH_MEASURE(0.001),#34852,
'DISTANCE_ACCURACY_VALUE',
'Maximum model space distance between geometric entities at asserted c
onnectivities');
#34757=UNCERTAINTY_MEASURE_WITH_UNIT(LENGTH_MEASURE(0.001),#34852,
'DISTANCE_ACCURACY_VALUE',
'Maximum model space distance between geometric entities at asserted c
onnectivities');
#34758=UNCERTAINTY_MEASURE_WITH_UNIT(LENGTH_MEASURE(0.001),#34852,
'DISTANCE_ACCURACY_VALUE',
'Maximum model space distance between geometric entities at asserted c
onnectivities');
#34759=UNCERTAINTY_MEASURE_WITH_UNIT(LENGTH_MEASURE(0.001),#34852,
'DISTANCE_ACCURACY_VALUE',
'Maximum model space distance between geometric entities at asserted c
onnectivities');
#34760=UNCERTAINTY_MEASURE_WITH_UNIT(LENGTH_MEASURE(0.001),#34852,
'DISTANCE_ACCURACY_VALUE',
'Maximum model space distance between geometric entities at asserted c
onnectivities');
#34761=UNCERTAINTY_MEASURE_WITH_UNIT(LENGTH_MEASURE(0.001),#34852,
'DISTANCE_ACCURACY_VALUE',
'Maximum model space distance between geometric entities at asserted c
onnectivities');
#34762=UNCERTAINTY_MEASURE_WITH_UNIT(LENGTH_MEASURE(0.001),#34852,
'DISTANCE_ACCURACY_VALUE',
'Maximum model space distance between geometric entities at asserted c
onnectivities');
#34763=UNCERTAINTY_MEASURE_WITH_UNIT(LENGTH_MEASURE(0.001),#34852,
'DISTANCE_ACCURACY_VALUE',
'Maximum model space distance between geometric entities at asserted c
onnectivities');
#34764=UNCERTAINTY_MEASURE_WITH_UNIT(LENGTH_MEASURE(0.001),#34852,
'DISTANCE_ACCURACY_VALUE',
'Maximum model space distance between geometric entities at asserted c
onnectivities');
#34765=UNCERTAINTY_MEASURE_WITH_UNIT(LENGTH_MEASURE(0.001),#34852,
'DISTANCE_ACCURACY_VALUE',
'Maximum model space distance between geometric entities at asserted c
onnectivities');
#34766=UNCERTAINTY_MEASURE_WITH_UNIT(LENGTH_MEASURE(0.001),#34852,
'DISTANCE_ACCURACY_VALUE',
'Maximum model space distance between geometric entities at asserted c
onnectivities');
#34767=UNCERTAINTY_MEASURE_WITH_UNIT(LENGTH_MEASURE(0.001),#34852,
'DISTANCE_ACCURACY_VALUE',
'Maximum model space distance between geometric entities at asserted c
onnectivities');
#34768=UNCERTAINTY_MEASURE_WITH_UNIT(LENGTH_MEASURE(0.001),#34852,
'DISTANCE_ACCURACY_VALUE',
'Maximum model space distance between geometric entities at asserted c
onnectivities');
#34769=UNCERTAINTY_MEASURE_WITH_UNIT(LENGTH_MEASURE(0.001),#34852,
'DISTANCE_ACCURACY_VALUE',
'Maximum model space distance between geometric entities at asserted c
onnectivities');
#34770=UNCERTAINTY_MEASURE_WITH_UNIT(LENGTH_MEASURE(0.001),#34852,
'DISTANCE_ACCURACY_VALUE',
'Maximum model space distance between geometric entities at asserted c
onnectivities');
#34771=UNCERTAINTY_MEASURE_WITH_UNIT(LENGTH_MEASURE(0.001),#34852,
'DISTANCE_ACCURACY_VALUE',
'Maximum model space distance between geometric entities at asserted c
onnectivities');
#34772=UNCERTAINTY_MEASURE_WITH_UNIT(LENGTH_MEASURE(0.001),#34852,
'DISTANCE_ACCURACY_VALUE',
'Maximum model space distance between geometric entities at asserted c
onnectivities');
#34773=UNCERTAINTY_MEASURE_WITH_UNIT(LENGTH_MEASURE(0.001),#34852,
'DISTANCE_ACCURACY_VALUE',
'Maximum model space distance between geometric entities at asserted c
onnectivities');
#34774=UNCERTAINTY_MEASURE_WITH_UNIT(LENGTH_MEASURE(0.001),#34852,
'DISTANCE_ACCURACY_VALUE',
'Maximum model space distance between geometric entities at asserted c
onnectivities');
#34775=UNCERTAINTY_MEASURE_WITH_UNIT(LENGTH_MEASURE(0.001),#34852,
'DISTANCE_ACCURACY_VALUE',
'Maximum model space distance between geometric entities at asserted c
onnectivities');
#34776=UNCERTAINTY_MEASURE_WITH_UNIT(LENGTH_MEASURE(0.001),#34852,
'DISTANCE_ACCURACY_VALUE',
'Maximum model space distance between geometric entities at asserted c
onnectivities');
#34777=UNCERTAINTY_MEASURE_WITH_UNIT(LENGTH_MEASURE(0.001),#34852,
'DISTANCE_ACCURACY_VALUE',
'Maximum model space distance between geometric entities at asserted c
onnectivities');
#34778=UNCERTAINTY_MEASURE_WITH_UNIT(LENGTH_MEASURE(0.001),#34852,
'DISTANCE_ACCURACY_VALUE',
'Maximum model space distance between geometric entities at asserted c
onnectivities');
#34779=UNCERTAINTY_MEASURE_WITH_UNIT(LENGTH_MEASURE(0.001),#34852,
'DISTANCE_ACCURACY_VALUE',
'Maximum model space distance between geometric entities at asserted c
onnectivities');
#34780=UNCERTAINTY_MEASURE_WITH_UNIT(LENGTH_MEASURE(0.001),#34852,
'DISTANCE_ACCURACY_VALUE',
'Maximum model space distance between geometric entities at asserted c
onnectivities');
#34781=UNCERTAINTY_MEASURE_WITH_UNIT(LENGTH_MEASURE(0.001),#34852,
'DISTANCE_ACCURACY_VALUE',
'Maximum model space distance between geometric entities at asserted c
onnectivities');
#34782=UNCERTAINTY_MEASURE_WITH_UNIT(LENGTH_MEASURE(0.001),#34852,
'DISTANCE_ACCURACY_VALUE',
'Maximum model space distance between geometric entities at asserted c
onnectivities');
#34783=UNCERTAINTY_MEASURE_WITH_UNIT(LENGTH_MEASURE(0.001),#34852,
'DISTANCE_ACCURACY_VALUE',
'Maximum model space distance between geometric entities at asserted c
onnectivities');
#34784=UNCERTAINTY_MEASURE_WITH_UNIT(LENGTH_MEASURE(0.001),#34852,
'DISTANCE_ACCURACY_VALUE',
'Maximum model space distance between geometric entities at asserted c
onnectivities');
#34785=UNCERTAINTY_MEASURE_WITH_UNIT(LENGTH_MEASURE(0.001),#34852,
'DISTANCE_ACCURACY_VALUE',
'Maximum model space distance between geometric entities at asserted c
onnectivities');
#34786=UNCERTAINTY_MEASURE_WITH_UNIT(LENGTH_MEASURE(0.001),#34852,
'DISTANCE_ACCURACY_VALUE',
'Maximum model space distance between geometric entities at asserted c
onnectivities');
#34787=UNCERTAINTY_MEASURE_WITH_UNIT(LENGTH_MEASURE(0.001),#34852,
'DISTANCE_ACCURACY_VALUE',
'Maximum model space distance between geometric entities at asserted c
onnectivities');
#34788=UNCERTAINTY_MEASURE_WITH_UNIT(LENGTH_MEASURE(0.001),#34852,
'DISTANCE_ACCURACY_VALUE',
'Maximum model space distance between geometric entities at asserted c
onnectivities');
#34789=UNCERTAINTY_MEASURE_WITH_UNIT(LENGTH_MEASURE(0.001),#34852,
'DISTANCE_ACCURACY_VALUE',
'Maximum model space distance between geometric entities at asserted c
onnectivities');
#34790=UNCERTAINTY_MEASURE_WITH_UNIT(LENGTH_MEASURE(0.001),#34852,
'DISTANCE_ACCURACY_VALUE',
'Maximum model space distance between geometric entities at asserted c
onnectivities');
#34791=UNCERTAINTY_MEASURE_WITH_UNIT(LENGTH_MEASURE(0.001),#34852,
'DISTANCE_ACCURACY_VALUE',
'Maximum model space distance between geometric entities at asserted c
onnectivities');
#34792=UNCERTAINTY_MEASURE_WITH_UNIT(LENGTH_MEASURE(0.001),#34852,
'DISTANCE_ACCURACY_VALUE',
'Maximum model space distance between geometric entities at asserted c
onnectivities');
#34793=UNCERTAINTY_MEASURE_WITH_UNIT(LENGTH_MEASURE(0.001),#34852,
'DISTANCE_ACCURACY_VALUE',
'Maximum model space distance between geometric entities at asserted c
onnectivities');
#34794=UNCERTAINTY_MEASURE_WITH_UNIT(LENGTH_MEASURE(0.001),#34852,
'DISTANCE_ACCURACY_VALUE',
'Maximum model space distance between geometric entities at asserted c
onnectivities');
#34795=UNCERTAINTY_MEASURE_WITH_UNIT(LENGTH_MEASURE(0.001),#34852,
'DISTANCE_ACCURACY_VALUE',
'Maximum model space distance between geometric entities at asserted c
onnectivities');
#34796=UNCERTAINTY_MEASURE_WITH_UNIT(LENGTH_MEASURE(0.001),#34852,
'DISTANCE_ACCURACY_VALUE',
'Maximum model space distance between geometric entities at asserted c
onnectivities');
#34797=UNCERTAINTY_MEASURE_WITH_UNIT(LENGTH_MEASURE(0.001),#34852,
'DISTANCE_ACCURACY_VALUE',
'Maximum model space distance between geometric entities at asserted c
onnectivities');
#34798=(
GEOMETRIC_REPRESENTATION_CONTEXT(3)
GLOBAL_UNCERTAINTY_ASSIGNED_CONTEXT((#34744))
GLOBAL_UNIT_ASSIGNED_CONTEXT((#34852,#34854,#34855))
REPRESENTATION_CONTEXT('','3D')
);
#34799=(
GEOMETRIC_REPRESENTATION_CONTEXT(3)
GLOBAL_UNCERTAINTY_ASSIGNED_CONTEXT((#34745))
GLOBAL_UNIT_ASSIGNED_CONTEXT((#34852,#34854,#34855))
REPRESENTATION_CONTEXT('','3D')
);
#34800=(
GEOMETRIC_REPRESENTATION_CONTEXT(3)
GLOBAL_UNCERTAINTY_ASSIGNED_CONTEXT((#34746))
GLOBAL_UNIT_ASSIGNED_CONTEXT((#34852,#34854,#34855))
REPRESENTATION_CONTEXT('','3D')
);
#34801=(
GEOMETRIC_REPRESENTATION_CONTEXT(3)
GLOBAL_UNCERTAINTY_ASSIGNED_CONTEXT((#34747))
GLOBAL_UNIT_ASSIGNED_CONTEXT((#34852,#34854,#34855))
REPRESENTATION_CONTEXT('','3D')
);
#34802=(
GEOMETRIC_REPRESENTATION_CONTEXT(3)
GLOBAL_UNCERTAINTY_ASSIGNED_CONTEXT((#34748))
GLOBAL_UNIT_ASSIGNED_CONTEXT((#34852,#34854,#34855))
REPRESENTATION_CONTEXT('','3D')
);
#34803=(
GEOMETRIC_REPRESENTATION_CONTEXT(3)
GLOBAL_UNCERTAINTY_ASSIGNED_CONTEXT((#34749))
GLOBAL_UNIT_ASSIGNED_CONTEXT((#34852,#34854,#34855))
REPRESENTATION_CONTEXT('','3D')
);
#34804=(
GEOMETRIC_REPRESENTATION_CONTEXT(3)
GLOBAL_UNCERTAINTY_ASSIGNED_CONTEXT((#34750))
GLOBAL_UNIT_ASSIGNED_CONTEXT((#34852,#34854,#34855))
REPRESENTATION_CONTEXT('','3D')
);
#34805=(
GEOMETRIC_REPRESENTATION_CONTEXT(3)
GLOBAL_UNCERTAINTY_ASSIGNED_CONTEXT((#34751))
GLOBAL_UNIT_ASSIGNED_CONTEXT((#34852,#34854,#34855))
REPRESENTATION_CONTEXT('','3D')
);
#34806=(
GEOMETRIC_REPRESENTATION_CONTEXT(3)
GLOBAL_UNCERTAINTY_ASSIGNED_CONTEXT((#34752))
GLOBAL_UNIT_ASSIGNED_CONTEXT((#34852,#34854,#34855))
REPRESENTATION_CONTEXT('','3D')
);
#34807=(
GEOMETRIC_REPRESENTATION_CONTEXT(3)
GLOBAL_UNCERTAINTY_ASSIGNED_CONTEXT((#34753))
GLOBAL_UNIT_ASSIGNED_CONTEXT((#34852,#34854,#34855))
REPRESENTATION_CONTEXT('','3D')
);
#34808=(
GEOMETRIC_REPRESENTATION_CONTEXT(3)
GLOBAL_UNCERTAINTY_ASSIGNED_CONTEXT((#34754))
GLOBAL_UNIT_ASSIGNED_CONTEXT((#34852,#34854,#34855))
REPRESENTATION_CONTEXT('','3D')
);
#34809=(
GEOMETRIC_REPRESENTATION_CONTEXT(3)
GLOBAL_UNCERTAINTY_ASSIGNED_CONTEXT((#34755))
GLOBAL_UNIT_ASSIGNED_CONTEXT((#34852,#34854,#34855))
REPRESENTATION_CONTEXT('','3D')
);
#34810=(
GEOMETRIC_REPRESENTATION_CONTEXT(3)
GLOBAL_UNCERTAINTY_ASSIGNED_CONTEXT((#34756))
GLOBAL_UNIT_ASSIGNED_CONTEXT((#34852,#34854,#34855))
REPRESENTATION_CONTEXT('','3D')
);
#34811=(
GEOMETRIC_REPRESENTATION_CONTEXT(3)
GLOBAL_UNCERTAINTY_ASSIGNED_CONTEXT((#34757))
GLOBAL_UNIT_ASSIGNED_CONTEXT((#34852,#34854,#34855))
REPRESENTATION_CONTEXT('','3D')
);
#34812=(
GEOMETRIC_REPRESENTATION_CONTEXT(3)
GLOBAL_UNCERTAINTY_ASSIGNED_CONTEXT((#34758))
GLOBAL_UNIT_ASSIGNED_CONTEXT((#34852,#34854,#34855))
REPRESENTATION_CONTEXT('','3D')
);
#34813=(
GEOMETRIC_REPRESENTATION_CONTEXT(3)
GLOBAL_UNCERTAINTY_ASSIGNED_CONTEXT((#34759))
GLOBAL_UNIT_ASSIGNED_CONTEXT((#34852,#34854,#34855))
REPRESENTATION_CONTEXT('','3D')
);
#34814=(
GEOMETRIC_REPRESENTATION_CONTEXT(3)
GLOBAL_UNCERTAINTY_ASSIGNED_CONTEXT((#34760))
GLOBAL_UNIT_ASSIGNED_CONTEXT((#34852,#34854,#34855))
REPRESENTATION_CONTEXT('','3D')
);
#34815=(
GEOMETRIC_REPRESENTATION_CONTEXT(3)
GLOBAL_UNCERTAINTY_ASSIGNED_CONTEXT((#34761))
GLOBAL_UNIT_ASSIGNED_CONTEXT((#34852,#34854,#34855))
REPRESENTATION_CONTEXT('','3D')
);
#34816=(
GEOMETRIC_REPRESENTATION_CONTEXT(3)
GLOBAL_UNCERTAINTY_ASSIGNED_CONTEXT((#34762))
GLOBAL_UNIT_ASSIGNED_CONTEXT((#34852,#34854,#34855))
REPRESENTATION_CONTEXT('','3D')
);
#34817=(
GEOMETRIC_REPRESENTATION_CONTEXT(3)
GLOBAL_UNCERTAINTY_ASSIGNED_CONTEXT((#34763))
GLOBAL_UNIT_ASSIGNED_CONTEXT((#34852,#34854,#34855))
REPRESENTATION_CONTEXT('','3D')
);
#34818=(
GEOMETRIC_REPRESENTATION_CONTEXT(3)
GLOBAL_UNCERTAINTY_ASSIGNED_CONTEXT((#34764))
GLOBAL_UNIT_ASSIGNED_CONTEXT((#34852,#34854,#34855))
REPRESENTATION_CONTEXT('','3D')
);
#34819=(
GEOMETRIC_REPRESENTATION_CONTEXT(3)
GLOBAL_UNCERTAINTY_ASSIGNED_CONTEXT((#34765))
GLOBAL_UNIT_ASSIGNED_CONTEXT((#34852,#34854,#34855))
REPRESENTATION_CONTEXT('','3D')
);
#34820=(
GEOMETRIC_REPRESENTATION_CONTEXT(3)
GLOBAL_UNCERTAINTY_ASSIGNED_CONTEXT((#34766))
GLOBAL_UNIT_ASSIGNED_CONTEXT((#34852,#34854,#34855))
REPRESENTATION_CONTEXT('','3D')
);
#34821=(
GEOMETRIC_REPRESENTATION_CONTEXT(3)
GLOBAL_UNCERTAINTY_ASSIGNED_CONTEXT((#34767))
GLOBAL_UNIT_ASSIGNED_CONTEXT((#34852,#34854,#34855))
REPRESENTATION_CONTEXT('','3D')
);
#34822=(
GEOMETRIC_REPRESENTATION_CONTEXT(3)
GLOBAL_UNCERTAINTY_ASSIGNED_CONTEXT((#34768))
GLOBAL_UNIT_ASSIGNED_CONTEXT((#34852,#34854,#34855))
REPRESENTATION_CONTEXT('','3D')
);
#34823=(
GEOMETRIC_REPRESENTATION_CONTEXT(3)
GLOBAL_UNCERTAINTY_ASSIGNED_CONTEXT((#34769))
GLOBAL_UNIT_ASSIGNED_CONTEXT((#34852,#34854,#34855))
REPRESENTATION_CONTEXT('','3D')
);
#34824=(
GEOMETRIC_REPRESENTATION_CONTEXT(3)
GLOBAL_UNCERTAINTY_ASSIGNED_CONTEXT((#34770))
GLOBAL_UNIT_ASSIGNED_CONTEXT((#34852,#34854,#34855))
REPRESENTATION_CONTEXT('','3D')
);
#34825=(
GEOMETRIC_REPRESENTATION_CONTEXT(3)
GLOBAL_UNCERTAINTY_ASSIGNED_CONTEXT((#34771))
GLOBAL_UNIT_ASSIGNED_CONTEXT((#34852,#34854,#34855))
REPRESENTATION_CONTEXT('','3D')
);
#34826=(
GEOMETRIC_REPRESENTATION_CONTEXT(3)
GLOBAL_UNCERTAINTY_ASSIGNED_CONTEXT((#34772))
GLOBAL_UNIT_ASSIGNED_CONTEXT((#34852,#34854,#34855))
REPRESENTATION_CONTEXT('','3D')
);
#34827=(
GEOMETRIC_REPRESENTATION_CONTEXT(3)
GLOBAL_UNCERTAINTY_ASSIGNED_CONTEXT((#34773))
GLOBAL_UNIT_ASSIGNED_CONTEXT((#34852,#34854,#34855))
REPRESENTATION_CONTEXT('','3D')
);
#34828=(
GEOMETRIC_REPRESENTATION_CONTEXT(3)
GLOBAL_UNCERTAINTY_ASSIGNED_CONTEXT((#34774))
GLOBAL_UNIT_ASSIGNED_CONTEXT((#34852,#34854,#34855))
REPRESENTATION_CONTEXT('','3D')
);
#34829=(
GEOMETRIC_REPRESENTATION_CONTEXT(3)
GLOBAL_UNCERTAINTY_ASSIGNED_CONTEXT((#34775))
GLOBAL_UNIT_ASSIGNED_CONTEXT((#34852,#34854,#34855))
REPRESENTATION_CONTEXT('','3D')
);
#34830=(
GEOMETRIC_REPRESENTATION_CONTEXT(3)
GLOBAL_UNCERTAINTY_ASSIGNED_CONTEXT((#34776))
GLOBAL_UNIT_ASSIGNED_CONTEXT((#34852,#34854,#34855))
REPRESENTATION_CONTEXT('','3D')
);
#34831=(
GEOMETRIC_REPRESENTATION_CONTEXT(3)
GLOBAL_UNCERTAINTY_ASSIGNED_CONTEXT((#34777))
GLOBAL_UNIT_ASSIGNED_CONTEXT((#34852,#34854,#34855))
REPRESENTATION_CONTEXT('','3D')
);
#34832=(
GEOMETRIC_REPRESENTATION_CONTEXT(3)
GLOBAL_UNCERTAINTY_ASSIGNED_CONTEXT((#34778))
GLOBAL_UNIT_ASSIGNED_CONTEXT((#34852,#34854,#34855))
REPRESENTATION_CONTEXT('','3D')
);
#34833=(
GEOMETRIC_REPRESENTATION_CONTEXT(3)
GLOBAL_UNCERTAINTY_ASSIGNED_CONTEXT((#34779))
GLOBAL_UNIT_ASSIGNED_CONTEXT((#34852,#34854,#34855))
REPRESENTATION_CONTEXT('','3D')
);
#34834=(
GEOMETRIC_REPRESENTATION_CONTEXT(3)
GLOBAL_UNCERTAINTY_ASSIGNED_CONTEXT((#34780))
GLOBAL_UNIT_ASSIGNED_CONTEXT((#34852,#34854,#34855))
REPRESENTATION_CONTEXT('','3D')
);
#34835=(
GEOMETRIC_REPRESENTATION_CONTEXT(3)
GLOBAL_UNCERTAINTY_ASSIGNED_CONTEXT((#34781))
GLOBAL_UNIT_ASSIGNED_CONTEXT((#34852,#34854,#34855))
REPRESENTATION_CONTEXT('','3D')
);
#34836=(
GEOMETRIC_REPRESENTATION_CONTEXT(3)
GLOBAL_UNCERTAINTY_ASSIGNED_CONTEXT((#34782))
GLOBAL_UNIT_ASSIGNED_CONTEXT((#34852,#34854,#34855))
REPRESENTATION_CONTEXT('','3D')
);
#34837=(
GEOMETRIC_REPRESENTATION_CONTEXT(3)
GLOBAL_UNCERTAINTY_ASSIGNED_CONTEXT((#34783))
GLOBAL_UNIT_ASSIGNED_CONTEXT((#34852,#34854,#34855))
REPRESENTATION_CONTEXT('','3D')
);
#34838=(
GEOMETRIC_REPRESENTATION_CONTEXT(3)
GLOBAL_UNCERTAINTY_ASSIGNED_CONTEXT((#34784))
GLOBAL_UNIT_ASSIGNED_CONTEXT((#34852,#34854,#34855))
REPRESENTATION_CONTEXT('','3D')
);
#34839=(
GEOMETRIC_REPRESENTATION_CONTEXT(3)
GLOBAL_UNCERTAINTY_ASSIGNED_CONTEXT((#34785))
GLOBAL_UNIT_ASSIGNED_CONTEXT((#34852,#34854,#34855))
REPRESENTATION_CONTEXT('','3D')
);
#34840=(
GEOMETRIC_REPRESENTATION_CONTEXT(3)
GLOBAL_UNCERTAINTY_ASSIGNED_CONTEXT((#34786))
GLOBAL_UNIT_ASSIGNED_CONTEXT((#34852,#34854,#34855))
REPRESENTATION_CONTEXT('','3D')
);
#34841=(
GEOMETRIC_REPRESENTATION_CONTEXT(3)
GLOBAL_UNCERTAINTY_ASSIGNED_CONTEXT((#34787))
GLOBAL_UNIT_ASSIGNED_CONTEXT((#34852,#34854,#34855))
REPRESENTATION_CONTEXT('','3D')
);
#34842=(
GEOMETRIC_REPRESENTATION_CONTEXT(3)
GLOBAL_UNCERTAINTY_ASSIGNED_CONTEXT((#34788))
GLOBAL_UNIT_ASSIGNED_CONTEXT((#34852,#34854,#34855))
REPRESENTATION_CONTEXT('','3D')
);
#34843=(
GEOMETRIC_REPRESENTATION_CONTEXT(3)
GLOBAL_UNCERTAINTY_ASSIGNED_CONTEXT((#34789))
GLOBAL_UNIT_ASSIGNED_CONTEXT((#34852,#34854,#34855))
REPRESENTATION_CONTEXT('','3D')
);
#34844=(
GEOMETRIC_REPRESENTATION_CONTEXT(3)
GLOBAL_UNCERTAINTY_ASSIGNED_CONTEXT((#34790))
GLOBAL_UNIT_ASSIGNED_CONTEXT((#34852,#34854,#34855))
REPRESENTATION_CONTEXT('','3D')
);
#34845=(
GEOMETRIC_REPRESENTATION_CONTEXT(3)
GLOBAL_UNCERTAINTY_ASSIGNED_CONTEXT((#34791))
GLOBAL_UNIT_ASSIGNED_CONTEXT((#34852,#34854,#34855))
REPRESENTATION_CONTEXT('','3D')
);
#34846=(
GEOMETRIC_REPRESENTATION_CONTEXT(3)
GLOBAL_UNCERTAINTY_ASSIGNED_CONTEXT((#34792))
GLOBAL_UNIT_ASSIGNED_CONTEXT((#34852,#34854,#34855))
REPRESENTATION_CONTEXT('','3D')
);
#34847=(
GEOMETRIC_REPRESENTATION_CONTEXT(3)
GLOBAL_UNCERTAINTY_ASSIGNED_CONTEXT((#34793))
GLOBAL_UNIT_ASSIGNED_CONTEXT((#34852,#34854,#34855))
REPRESENTATION_CONTEXT('','3D')
);
#34848=(
GEOMETRIC_REPRESENTATION_CONTEXT(3)
GLOBAL_UNCERTAINTY_ASSIGNED_CONTEXT((#34794))
GLOBAL_UNIT_ASSIGNED_CONTEXT((#34852,#34854,#34855))
REPRESENTATION_CONTEXT('','3D')
);
#34849=(
GEOMETRIC_REPRESENTATION_CONTEXT(3)
GLOBAL_UNCERTAINTY_ASSIGNED_CONTEXT((#34795))
GLOBAL_UNIT_ASSIGNED_CONTEXT((#34852,#34854,#34855))
REPRESENTATION_CONTEXT('','3D')
);
#34850=(
GEOMETRIC_REPRESENTATION_CONTEXT(3)
GLOBAL_UNCERTAINTY_ASSIGNED_CONTEXT((#34796))
GLOBAL_UNIT_ASSIGNED_CONTEXT((#34852,#34854,#34855))
REPRESENTATION_CONTEXT('','3D')
);
#34851=(
GEOMETRIC_REPRESENTATION_CONTEXT(3)
GLOBAL_UNCERTAINTY_ASSIGNED_CONTEXT((#34797))
GLOBAL_UNIT_ASSIGNED_CONTEXT((#34852,#34854,#34855))
REPRESENTATION_CONTEXT('','3D')
);
#34852=(
LENGTH_UNIT()
NAMED_UNIT(*)
SI_UNIT(.CENTI.,.METRE.)
);
#34853=(
LENGTH_UNIT()
NAMED_UNIT(*)
SI_UNIT($,.METRE.)
);
#34854=(
NAMED_UNIT(*)
PLANE_ANGLE_UNIT()
SI_UNIT($,.RADIAN.)
);
#34855=(
NAMED_UNIT(*)
SI_UNIT($,.STERADIAN.)
SOLID_ANGLE_UNIT()
);
#34856=SHAPE_DEFINITION_REPRESENTATION(#34909,#35073);
#34857=SHAPE_DEFINITION_REPRESENTATION(#34910,#35074);
#34858=SHAPE_DEFINITION_REPRESENTATION(#34911,#35075);
#34859=SHAPE_DEFINITION_REPRESENTATION(#34912,#35076);
#34860=SHAPE_DEFINITION_REPRESENTATION(#34913,#35077);
#34861=SHAPE_DEFINITION_REPRESENTATION(#34914,#35078);
#34862=SHAPE_DEFINITION_REPRESENTATION(#34915,#35079);
#34863=SHAPE_DEFINITION_REPRESENTATION(#34916,#35080);
#34864=SHAPE_DEFINITION_REPRESENTATION(#34917,#35081);
#34865=SHAPE_DEFINITION_REPRESENTATION(#34918,#35082);
#34866=SHAPE_DEFINITION_REPRESENTATION(#34919,#35083);
#34867=SHAPE_DEFINITION_REPRESENTATION(#34920,#35084);
#34868=SHAPE_DEFINITION_REPRESENTATION(#34921,#35085);
#34869=SHAPE_DEFINITION_REPRESENTATION(#34922,#35086);
#34870=SHAPE_DEFINITION_REPRESENTATION(#34923,#35087);
#34871=SHAPE_DEFINITION_REPRESENTATION(#34924,#35088);
#34872=SHAPE_DEFINITION_REPRESENTATION(#34925,#35089);
#34873=SHAPE_DEFINITION_REPRESENTATION(#34926,#35090);
#34874=SHAPE_DEFINITION_REPRESENTATION(#34927,#35091);
#34875=SHAPE_DEFINITION_REPRESENTATION(#34928,#35092);
#34876=SHAPE_DEFINITION_REPRESENTATION(#34929,#35093);
#34877=SHAPE_DEFINITION_REPRESENTATION(#34930,#35094);
#34878=SHAPE_DEFINITION_REPRESENTATION(#34931,#35095);
#34879=SHAPE_DEFINITION_REPRESENTATION(#34932,#35096);
#34880=SHAPE_DEFINITION_REPRESENTATION(#34933,#35097);
#34881=SHAPE_DEFINITION_REPRESENTATION(#34934,#35098);
#34882=SHAPE_DEFINITION_REPRESENTATION(#34935,#35099);
#34883=SHAPE_DEFINITION_REPRESENTATION(#34941,#35100);
#34884=SHAPE_DEFINITION_REPRESENTATION(#34942,#35101);
#34885=SHAPE_DEFINITION_REPRESENTATION(#34943,#35102);
#34886=SHAPE_DEFINITION_REPRESENTATION(#34944,#35103);
#34887=SHAPE_DEFINITION_REPRESENTATION(#34945,#35104);
#34888=SHAPE_DEFINITION_REPRESENTATION(#34946,#35105);
#34889=SHAPE_DEFINITION_REPRESENTATION(#34947,#35106);
#34890=SHAPE_DEFINITION_REPRESENTATION(#34948,#35107);
#34891=SHAPE_DEFINITION_REPRESENTATION(#34952,#35108);
#34892=SHAPE_DEFINITION_REPRESENTATION(#34953,#35109);
#34893=SHAPE_DEFINITION_REPRESENTATION(#34954,#35110);
#34894=SHAPE_DEFINITION_REPRESENTATION(#34955,#35111);
#34895=SHAPE_DEFINITION_REPRESENTATION(#34956,#35112);
#34896=SHAPE_DEFINITION_REPRESENTATION(#34957,#35113);
#34897=SHAPE_DEFINITION_REPRESENTATION(#34958,#35114);
#34898=SHAPE_DEFINITION_REPRESENTATION(#34959,#35115);
#34899=SHAPE_DEFINITION_REPRESENTATION(#34960,#35116);
#34900=SHAPE_DEFINITION_REPRESENTATION(#34961,#35117);
#34901=SHAPE_DEFINITION_REPRESENTATION(#34962,#35118);
#34902=SHAPE_DEFINITION_REPRESENTATION(#34963,#35119);
#34903=SHAPE_DEFINITION_REPRESENTATION(#34964,#35120);
#34904=SHAPE_DEFINITION_REPRESENTATION(#35047,#35121);
#34905=SHAPE_DEFINITION_REPRESENTATION(#35048,#35122);
#34906=SHAPE_DEFINITION_REPRESENTATION(#35049,#35123);
#34907=SHAPE_DEFINITION_REPRESENTATION(#35066,#35124);
#34908=SHAPE_DEFINITION_REPRESENTATION(#35067,#35125);
#34909=PRODUCT_DEFINITION_SHAPE('',$,#35127);
#34910=PRODUCT_DEFINITION_SHAPE('',$,#35128);
#34911=PRODUCT_DEFINITION_SHAPE('',$,#35129);
#34912=PRODUCT_DEFINITION_SHAPE('',$,#35130);
#34913=PRODUCT_DEFINITION_SHAPE('',$,#35131);
#34914=PRODUCT_DEFINITION_SHAPE('',$,#35132);
#34915=PRODUCT_DEFINITION_SHAPE('',$,#35133);
#34916=PRODUCT_DEFINITION_SHAPE('',$,#35134);
#34917=PRODUCT_DEFINITION_SHAPE('',$,#35135);
#34918=PRODUCT_DEFINITION_SHAPE('',$,#35136);
#34919=PRODUCT_DEFINITION_SHAPE('',$,#35137);
#34920=PRODUCT_DEFINITION_SHAPE('',$,#35138);
#34921=PRODUCT_DEFINITION_SHAPE('',$,#35139);
#34922=PRODUCT_DEFINITION_SHAPE('',$,#35140);
#34923=PRODUCT_DEFINITION_SHAPE('',$,#35141);
#34924=PRODUCT_DEFINITION_SHAPE('',$,#35142);
#34925=PRODUCT_DEFINITION_SHAPE('',$,#35143);
#34926=PRODUCT_DEFINITION_SHAPE('',$,#35144);
#34927=PRODUCT_DEFINITION_SHAPE('',$,#35145);
#34928=PRODUCT_DEFINITION_SHAPE('',$,#35146);
#34929=PRODUCT_DEFINITION_SHAPE('',$,#35147);
#34930=PRODUCT_DEFINITION_SHAPE('',$,#35148);
#34931=PRODUCT_DEFINITION_SHAPE('',$,#35149);
#34932=PRODUCT_DEFINITION_SHAPE('',$,#35150);
#34933=PRODUCT_DEFINITION_SHAPE('',$,#35151);
#34934=PRODUCT_DEFINITION_SHAPE('',$,#35152);
#34935=PRODUCT_DEFINITION_SHAPE('',$,#35153);
#34936=PRODUCT_DEFINITION_SHAPE($,$,#464);
#34937=PRODUCT_DEFINITION_SHAPE($,$,#465);
#34938=PRODUCT_DEFINITION_SHAPE($,$,#466);
#34939=PRODUCT_DEFINITION_SHAPE($,$,#467);
#34940=PRODUCT_DEFINITION_SHAPE($,$,#468);
#34941=PRODUCT_DEFINITION_SHAPE('',$,#35154);
#34942=PRODUCT_DEFINITION_SHAPE('',$,#35155);
#34943=PRODUCT_DEFINITION_SHAPE('',$,#35156);
#34944=PRODUCT_DEFINITION_SHAPE('',$,#35157);
#34945=PRODUCT_DEFINITION_SHAPE('',$,#35158);
#34946=PRODUCT_DEFINITION_SHAPE('',$,#35159);
#34947=PRODUCT_DEFINITION_SHAPE('',$,#35160);
#34948=PRODUCT_DEFINITION_SHAPE('',$,#35161);
#34949=PRODUCT_DEFINITION_SHAPE($,$,#469);
#34950=PRODUCT_DEFINITION_SHAPE($,$,#470);
#34951=PRODUCT_DEFINITION_SHAPE($,$,#471);
#34952=PRODUCT_DEFINITION_SHAPE('',$,#35162);
#34953=PRODUCT_DEFINITION_SHAPE('',$,#35163);
#34954=PRODUCT_DEFINITION_SHAPE('',$,#35164);
#34955=PRODUCT_DEFINITION_SHAPE('',$,#35165);
#34956=PRODUCT_DEFINITION_SHAPE('',$,#35166);
#34957=PRODUCT_DEFINITION_SHAPE('',$,#35167);
#34958=PRODUCT_DEFINITION_SHAPE('',$,#35168);
#34959=PRODUCT_DEFINITION_SHAPE('',$,#35169);
#34960=PRODUCT_DEFINITION_SHAPE('',$,#35170);
#34961=PRODUCT_DEFINITION_SHAPE('',$,#35171);
#34962=PRODUCT_DEFINITION_SHAPE('',$,#35172);
#34963=PRODUCT_DEFINITION_SHAPE('',$,#35173);
#34964=PRODUCT_DEFINITION_SHAPE('',$,#35174);
#34965=PRODUCT_DEFINITION_SHAPE($,$,#472);
#34966=PRODUCT_DEFINITION_SHAPE($,$,#473);
#34967=PRODUCT_DEFINITION_SHAPE($,$,#474);
#34968=PRODUCT_DEFINITION_SHAPE($,$,#475);
#34969=PRODUCT_DEFINITION_SHAPE($,$,#476);
#34970=PRODUCT_DEFINITION_SHAPE($,$,#477);
#34971=PRODUCT_DEFINITION_SHAPE($,$,#478);
#34972=PRODUCT_DEFINITION_SHAPE($,$,#479);
#34973=PRODUCT_DEFINITION_SHAPE($,$,#480);
#34974=PRODUCT_DEFINITION_SHAPE($,$,#481);
#34975=PRODUCT_DEFINITION_SHAPE($,$,#482);
#34976=PRODUCT_DEFINITION_SHAPE($,$,#483);
#34977=PRODUCT_DEFINITION_SHAPE($,$,#484);
#34978=PRODUCT_DEFINITION_SHAPE($,$,#485);
#34979=PRODUCT_DEFINITION_SHAPE($,$,#486);
#34980=PRODUCT_DEFINITION_SHAPE($,$,#487);
#34981=PRODUCT_DEFINITION_SHAPE($,$,#488);
#34982=PRODUCT_DEFINITION_SHAPE($,$,#489);
#34983=PRODUCT_DEFINITION_SHAPE($,$,#490);
#34984=PRODUCT_DEFINITION_SHAPE($,$,#491);
#34985=PRODUCT_DEFINITION_SHAPE($,$,#492);
#34986=PRODUCT_DEFINITION_SHAPE($,$,#493);
#34987=PRODUCT_DEFINITION_SHAPE($,$,#494);
#34988=PRODUCT_DEFINITION_SHAPE($,$,#495);
#34989=PRODUCT_DEFINITION_SHAPE($,$,#496);
#34990=PRODUCT_DEFINITION_SHAPE($,$,#497);
#34991=PRODUCT_DEFINITION_SHAPE($,$,#498);
#34992=PRODUCT_DEFINITION_SHAPE($,$,#499);
#34993=PRODUCT_DEFINITION_SHAPE($,$,#500);
#34994=PRODUCT_DEFINITION_SHAPE($,$,#501);
#34995=PRODUCT_DEFINITION_SHAPE($,$,#502);
#34996=PRODUCT_DEFINITION_SHAPE($,$,#503);
#34997=PRODUCT_DEFINITION_SHAPE($,$,#504);
#34998=PRODUCT_DEFINITION_SHAPE($,$,#505);
#34999=PRODUCT_DEFINITION_SHAPE($,$,#506);
#35000=PRODUCT_DEFINITION_SHAPE($,$,#507);
#35001=PRODUCT_DEFINITION_SHAPE($,$,#508);
#35002=PRODUCT_DEFINITION_SHAPE($,$,#509);
#35003=PRODUCT_DEFINITION_SHAPE($,$,#510);
#35004=PRODUCT_DEFINITION_SHAPE($,$,#511);
#35005=PRODUCT_DEFINITION_SHAPE($,$,#512);
#35006=PRODUCT_DEFINITION_SHAPE($,$,#513);
#35007=PRODUCT_DEFINITION_SHAPE($,$,#514);
#35008=PRODUCT_DEFINITION_SHAPE($,$,#515);
#35009=PRODUCT_DEFINITION_SHAPE($,$,#516);
#35010=PRODUCT_DEFINITION_SHAPE($,$,#517);
#35011=PRODUCT_DEFINITION_SHAPE($,$,#518);
#35012=PRODUCT_DEFINITION_SHAPE($,$,#519);
#35013=PRODUCT_DEFINITION_SHAPE($,$,#520);
#35014=PRODUCT_DEFINITION_SHAPE($,$,#521);
#35015=PRODUCT_DEFINITION_SHAPE($,$,#522);
#35016=PRODUCT_DEFINITION_SHAPE($,$,#523);
#35017=PRODUCT_DEFINITION_SHAPE($,$,#524);
#35018=PRODUCT_DEFINITION_SHAPE($,$,#525);
#35019=PRODUCT_DEFINITION_SHAPE($,$,#526);
#35020=PRODUCT_DEFINITION_SHAPE($,$,#527);
#35021=PRODUCT_DEFINITION_SHAPE($,$,#528);
#35022=PRODUCT_DEFINITION_SHAPE($,$,#529);
#35023=PRODUCT_DEFINITION_SHAPE($,$,#530);
#35024=PRODUCT_DEFINITION_SHAPE($,$,#531);
#35025=PRODUCT_DEFINITION_SHAPE($,$,#532);
#35026=PRODUCT_DEFINITION_SHAPE($,$,#533);
#35027=PRODUCT_DEFINITION_SHAPE($,$,#534);
#35028=PRODUCT_DEFINITION_SHAPE($,$,#535);
#35029=PRODUCT_DEFINITION_SHAPE($,$,#536);
#35030=PRODUCT_DEFINITION_SHAPE($,$,#537);
#35031=PRODUCT_DEFINITION_SHAPE($,$,#538);
#35032=PRODUCT_DEFINITION_SHAPE($,$,#539);
#35033=PRODUCT_DEFINITION_SHAPE($,$,#540);
#35034=PRODUCT_DEFINITION_SHAPE($,$,#541);
#35035=PRODUCT_DEFINITION_SHAPE($,$,#542);
#35036=PRODUCT_DEFINITION_SHAPE($,$,#543);
#35037=PRODUCT_DEFINITION_SHAPE($,$,#544);
#35038=PRODUCT_DEFINITION_SHAPE($,$,#545);
#35039=PRODUCT_DEFINITION_SHAPE($,$,#546);
#35040=PRODUCT_DEFINITION_SHAPE($,$,#547);
#35041=PRODUCT_DEFINITION_SHAPE($,$,#548);
#35042=PRODUCT_DEFINITION_SHAPE($,$,#549);
#35043=PRODUCT_DEFINITION_SHAPE($,$,#550);
#35044=PRODUCT_DEFINITION_SHAPE($,$,#551);
#35045=PRODUCT_DEFINITION_SHAPE($,$,#552);
#35046=PRODUCT_DEFINITION_SHAPE($,$,#553);
#35047=PRODUCT_DEFINITION_SHAPE('',$,#35175);
#35048=PRODUCT_DEFINITION_SHAPE('',$,#35176);
#35049=PRODUCT_DEFINITION_SHAPE('',$,#35177);
#35050=PRODUCT_DEFINITION_SHAPE($,$,#554);
#35051=PRODUCT_DEFINITION_SHAPE($,$,#555);
#35052=PRODUCT_DEFINITION_SHAPE($,$,#556);
#35053=PRODUCT_DEFINITION_SHAPE($,$,#557);
#35054=PRODUCT_DEFINITION_SHAPE($,$,#558);
#35055=PRODUCT_DEFINITION_SHAPE($,$,#559);
#35056=PRODUCT_DEFINITION_SHAPE($,$,#560);
#35057=PRODUCT_DEFINITION_SHAPE($,$,#561);
#35058=PRODUCT_DEFINITION_SHAPE($,$,#562);
#35059=PRODUCT_DEFINITION_SHAPE($,$,#563);
#35060=PRODUCT_DEFINITION_SHAPE($,$,#564);
#35061=PRODUCT_DEFINITION_SHAPE($,$,#565);
#35062=PRODUCT_DEFINITION_SHAPE($,$,#566);
#35063=PRODUCT_DEFINITION_SHAPE($,$,#567);
#35064=PRODUCT_DEFINITION_SHAPE($,$,#568);
#35065=PRODUCT_DEFINITION_SHAPE($,$,#569);
#35066=PRODUCT_DEFINITION_SHAPE('',$,#35178);
#35067=PRODUCT_DEFINITION_SHAPE('',$,#35179);
#35068=PRODUCT_DEFINITION_SHAPE($,$,#570);
#35069=PRODUCT_DEFINITION_SHAPE($,$,#571);
#35070=PRODUCT_DEFINITION_SHAPE($,$,#572);
#35071=PRODUCT_DEFINITION_SHAPE($,$,#573);
#35072=PRODUCT_DEFINITION_SHAPE($,$,#574);
#35073=SHAPE_REPRESENTATION('',(#14317,#15596,#15597,#15598,#15599),#34798);
#35074=SHAPE_REPRESENTATION('',(#14318,#15441,#15442,#15443,#15444,#15445,
#15446,#15447,#15448,#15449,#15450,#15451,#15452,#15453,#15454,#15455,#15456,
#15457,#15458,#15459,#15460,#15461,#15462,#15463,#15464,#15465,#15466,#15467,
#15468,#15469,#15470,#15471,#15472,#15473,#15474,#15475,#15476,#15477,#15478,
#15479,#15480,#15481,#15482,#15483,#15484,#15485,#15486,#15487,#15488,#15489,
#15490,#15491,#15492,#15493,#15494,#15495,#15496,#15497,#15498,#15499,#15500,
#15501,#15502,#15503,#15504,#15505,#15506,#15507,#15508,#15509,#15510,#15511),
#34799);
#35075=SHAPE_REPRESENTATION('',(#14319),#34800);
#35076=SHAPE_REPRESENTATION('',(#14338),#34801);
#35077=SHAPE_REPRESENTATION('',(#14345),#34802);
#35078=SHAPE_REPRESENTATION('',(#14352),#34803);
#35079=SHAPE_REPRESENTATION('',(#14407),#34804);
#35080=SHAPE_REPRESENTATION('',(#14428),#34805);
#35081=SHAPE_REPRESENTATION('',(#14435),#34806);
#35082=SHAPE_REPRESENTATION('',(#14456),#34807);
#35083=SHAPE_REPRESENTATION('',(#14463),#34808);
#35084=SHAPE_REPRESENTATION('',(#14495),#34809);
#35085=SHAPE_REPRESENTATION('',(#14520),#34810);
#35086=SHAPE_REPRESENTATION('',(#14545),#34811);
#35087=SHAPE_REPRESENTATION('',(#14577),#34812);
#35088=SHAPE_REPRESENTATION('',(#14602),#34813);
#35089=SHAPE_REPRESENTATION('',(#14627),#34814);
#35090=SHAPE_REPRESENTATION('',(#14677),#34815);
#35091=SHAPE_REPRESENTATION('',(#14698),#34816);
#35092=SHAPE_REPRESENTATION('',(#14709),#34817);
#35093=SHAPE_REPRESENTATION('',(#14752),#34818);
#35094=SHAPE_REPRESENTATION('',(#14778,#14901,#14902,#14903,#14904,#14905),
#34819);
#35095=SHAPE_REPRESENTATION('',(#14779),#34820);
#35096=SHAPE_REPRESENTATION('',(#14799),#34821);
#35097=SHAPE_REPRESENTATION('',(#14819),#34822);
#35098=SHAPE_REPRESENTATION('',(#14834),#34823);
#35099=SHAPE_REPRESENTATION('',(#14884),#34824);
#35100=SHAPE_REPRESENTATION('',(#14906),#34825);
#35101=SHAPE_REPRESENTATION('',(#14930,#15512,#15513,#15514,#15515,#15516,
#15517,#15518,#15519,#15520,#15521,#15522),#34826);
#35102=SHAPE_REPRESENTATION('',(#14931),#34827);
#35103=SHAPE_REPRESENTATION('',(#14962),#34828);
#35104=SHAPE_REPRESENTATION('',(#15109,#15171,#15172,#15173),#34829);
#35105=SHAPE_REPRESENTATION('',(#15110),#34830);
#35106=SHAPE_REPRESENTATION('',(#15149),#34831);
#35107=SHAPE_REPRESENTATION('',(#15160),#34832);
#35108=SHAPE_REPRESENTATION('',(#15174),#34833);
#35109=SHAPE_REPRESENTATION('',(#15198,#15569,#15570,#15571,#15572,#15573,
#15574,#15575,#15576,#15577,#15578,#15579,#15580,#15581,#15582,#15583,#15584),
#34834);
#35110=SHAPE_REPRESENTATION('',(#15199),#34835);
#35111=SHAPE_REPRESENTATION('',(#15235),#34836);
#35112=SHAPE_REPRESENTATION('',(#15244),#34837);
#35113=SHAPE_REPRESENTATION('',(#15253),#34838);
#35114=SHAPE_REPRESENTATION('',(#15262),#34839);
#35115=SHAPE_REPRESENTATION('',(#15271),#34840);
#35116=SHAPE_REPRESENTATION('',(#15280),#34841);
#35117=SHAPE_REPRESENTATION('',(#15289),#34842);
#35118=SHAPE_REPRESENTATION('',(#15313),#34843);
#35119=SHAPE_REPRESENTATION('',(#15322),#34844);
#35120=SHAPE_REPRESENTATION('',(#15415),#34845);
#35121=SHAPE_REPRESENTATION('',(#15523),#34846);
#35122=SHAPE_REPRESENTATION('',(#15534),#34847);
#35123=SHAPE_REPRESENTATION('',(#15543),#34848);
#35124=SHAPE_REPRESENTATION('',(#15585,#15595),#34849);
#35125=SHAPE_REPRESENTATION('',(#15586),#34850);
#35126=PRODUCT_DEFINITION_CONTEXT('part definition',#35287,'design');
#35127=PRODUCT_DEFINITION('PAT-085','PAT-085',#35180,
#35126);
#35128=PRODUCT_DEFINITION('Extrusion frame and pinion bearings',
'Extrusion frame and pinion bearings',#35181,#35126);
#35129=PRODUCT_DEFINITION('Base','Base',#35182,#35126);
#35130=PRODUCT_DEFINITION('Foot strip','Foot strip',#35183,#35126);
#35131=PRODUCT_DEFINITION('Foot strip (1)','Foot strip (1)',#35184,#35126);
#35132=PRODUCT_DEFINITION('Rail support plate','Rail support plate',#35185,
#35126);
#35133=PRODUCT_DEFINITION('End stop','End stop',#35186,#35126);
#35134=PRODUCT_DEFINITION('End bumper','End bumper',#35187,#35126);
#35135=PRODUCT_DEFINITION('End stop (1)','End stop (1)',#35188,#35126);
#35136=PRODUCT_DEFINITION('End bumper (1)','End bumper (1)',#35189,#35126);
#35137=PRODUCT_DEFINITION('Pinion bearing pedestal',
'Pinion bearing pedestal',#35190,#35126);
#35138=PRODUCT_DEFINITION('Bearing cap','Bearing cap',#35191,#35126);
#35139=PRODUCT_DEFINITION('Bearing cap (1)','Bearing cap (1)',#35192,#35126);
#35140=PRODUCT_DEFINITION('Pinion bearing pedestal (1)',
'Pinion bearing pedestal (1)',#35193,#35126);
#35141=PRODUCT_DEFINITION('Bearing cap (2)','Bearing cap (2)',#35194,#35126);
#35142=PRODUCT_DEFINITION('Bearing cap (3)','Bearing cap (3)',#35195,#35126);
#35143=PRODUCT_DEFINITION('Slotted Extrusion - 20 x 20 x 200 mm',
'Slotted Extrusion - 20 x 20 x 200 mm',#35196,#35126);
#35144=PRODUCT_DEFINITION('Captive slot nut','Captive slot nut',#35197,
#35126);
#35145=PRODUCT_DEFINITION('Flat Washer - M5','Flat Washer - M5',#35198,
#35126);
#35146=PRODUCT_DEFINITION('Linear Guide Rail - 15 mm, 220 mm Long',
'Linear Guide Rail - 15 mm, 220 mm Long',#35199,#35126);
#35147=PRODUCT_DEFINITION('Cap Screw - M5x20','Cap Screw - M5x20',#35200,
#35126);
#35148=PRODUCT_DEFINITION('Sealed Ball Bearing - 12 x 32 x 10 mm',
'Sealed Ball Bearing - 12 x 32 x 10 mm',#35201,#35126);
#35149=PRODUCT_DEFINITION('Inner ring','Inner ring',#35202,#35126);
#35150=PRODUCT_DEFINITION('Outer ring','Outer ring',#35203,#35126);
#35151=PRODUCT_DEFINITION('Balls','Balls',#35204,#35126);
#35152=PRODUCT_DEFINITION('Cage','Cage',#35205,#35126);
#35153=PRODUCT_DEFINITION('Seals 2RS','Seals 2RS',#35206,#35126);
#35154=PRODUCT_DEFINITION('M4x10 Cap Screw','M4x10 Cap Screw',#35207,#35126);
#35155=PRODUCT_DEFINITION('Rack and carriage','Rack and carriage',#35208,
#35126);
#35156=PRODUCT_DEFINITION('Table','Table',#35209,#35126);
#35157=PRODUCT_DEFINITION('Module 2 rack','Module 2 rack',#35210,#35126);
#35158=PRODUCT_DEFINITION('Flanged Linear Guide Carriage - 15 mm',
'Flanged Linear Guide Carriage - 15 mm',#35211,#35126);
#35159=PRODUCT_DEFINITION('Block','Block',#35212,#35126);
#35160=PRODUCT_DEFINITION('End cap +','End cap +',#35213,#35126);
#35161=PRODUCT_DEFINITION('End cap','End cap',#35214,#35126);
#35162=PRODUCT_DEFINITION('M5x14 Cap Screw','M5x14 Cap Screw',#35215,#35126);
#35163=PRODUCT_DEFINITION('Pinion shaft and crank',
'Pinion shaft and crank',#35216,#35126);
#35164=PRODUCT_DEFINITION('Pinion shaft','Pinion shaft',#35217,#35126);
#35165=PRODUCT_DEFINITION('Gear front spacer','Gear front spacer',#35218,
#35126);
#35166=PRODUCT_DEFINITION('Rear inner spacer','Rear inner spacer',#35219,
#35126);
#35167=PRODUCT_DEFINITION('Crank inner spacer','Crank inner spacer',#35220,
#35126);
#35168=PRODUCT_DEFINITION('Shaft keeper','Shaft keeper',#35221,#35126);
#35169=PRODUCT_DEFINITION('Shaft keeper (1)','Shaft keeper (1)',#35222,#35126);
#35170=PRODUCT_DEFINITION('Rear end sleeve','Rear end sleeve',#35223,#35126);
#35171=PRODUCT_DEFINITION('Crank','Crank',#35224,#35126);
#35172=PRODUCT_DEFINITION('Grip bushing','Grip bushing',#35225,#35126);
#35173=PRODUCT_DEFINITION('Spur Gear - Module 2, 20 Teeth, 12 mm Bore',
'Spur Gear - Module 2, 20 Teeth, 12 mm Bore',#35226,#35126);
#35174=PRODUCT_DEFINITION('Cap Screw - M4x16','Cap Screw - M4x16',#35227,
#35126);
#35175=PRODUCT_DEFINITION('Key 4x4x14','Key 4x4x14',#35228,#35126);
#35176=PRODUCT_DEFINITION('Flat Washer - M6','Flat Washer - M6',#35229,
#35126);
#35177=PRODUCT_DEFINITION('Cap Screw - M6x25','Cap Screw - M6x25',#35230,
#35126);
#35178=PRODUCT_DEFINITION('Revolving grip','Revolving grip',#35231,#35126);
#35179=PRODUCT_DEFINITION('Handle','Handle',#35232,#35126);
#35180=PRODUCT_DEFINITION_FORMATION('',$,#35289);
#35181=PRODUCT_DEFINITION_FORMATION('',$,#35290);
#35182=PRODUCT_DEFINITION_FORMATION('',$,#35291);
#35183=PRODUCT_DEFINITION_FORMATION('',$,#35292);
#35184=PRODUCT_DEFINITION_FORMATION('',$,#35293);
#35185=PRODUCT_DEFINITION_FORMATION('',$,#35294);
#35186=PRODUCT_DEFINITION_FORMATION('',$,#35295);
#35187=PRODUCT_DEFINITION_FORMATION('',$,#35296);
#35188=PRODUCT_DEFINITION_FORMATION('',$,#35297);
#35189=PRODUCT_DEFINITION_FORMATION('',$,#35298);
#35190=PRODUCT_DEFINITION_FORMATION('',$,#35299);
#35191=PRODUCT_DEFINITION_FORMATION('',$,#35300);
#35192=PRODUCT_DEFINITION_FORMATION('',$,#35301);
#35193=PRODUCT_DEFINITION_FORMATION('',$,#35302);
#35194=PRODUCT_DEFINITION_FORMATION('',$,#35303);
#35195=PRODUCT_DEFINITION_FORMATION('',$,#35304);
#35196=PRODUCT_DEFINITION_FORMATION('',$,#35305);
#35197=PRODUCT_DEFINITION_FORMATION('',$,#35306);
#35198=PRODUCT_DEFINITION_FORMATION('',$,#35307);
#35199=PRODUCT_DEFINITION_FORMATION('',$,#35308);
#35200=PRODUCT_DEFINITION_FORMATION('',$,#35309);
#35201=PRODUCT_DEFINITION_FORMATION('',$,#35310);
#35202=PRODUCT_DEFINITION_FORMATION('',$,#35311);
#35203=PRODUCT_DEFINITION_FORMATION('',$,#35312);
#35204=PRODUCT_DEFINITION_FORMATION('',$,#35313);
#35205=PRODUCT_DEFINITION_FORMATION('',$,#35314);
#35206=PRODUCT_DEFINITION_FORMATION('',$,#35315);
#35207=PRODUCT_DEFINITION_FORMATION('',$,#35316);
#35208=PRODUCT_DEFINITION_FORMATION('',$,#35317);
#35209=PRODUCT_DEFINITION_FORMATION('',$,#35318);
#35210=PRODUCT_DEFINITION_FORMATION('',$,#35319);
#35211=PRODUCT_DEFINITION_FORMATION('',$,#35320);
#35212=PRODUCT_DEFINITION_FORMATION('',$,#35321);
#35213=PRODUCT_DEFINITION_FORMATION('',$,#35322);
#35214=PRODUCT_DEFINITION_FORMATION('',$,#35323);
#35215=PRODUCT_DEFINITION_FORMATION('',$,#35324);
#35216=PRODUCT_DEFINITION_FORMATION('',$,#35325);
#35217=PRODUCT_DEFINITION_FORMATION('',$,#35326);
#35218=PRODUCT_DEFINITION_FORMATION('',$,#35327);
#35219=PRODUCT_DEFINITION_FORMATION('',$,#35328);
#35220=PRODUCT_DEFINITION_FORMATION('',$,#35329);
#35221=PRODUCT_DEFINITION_FORMATION('',$,#35330);
#35222=PRODUCT_DEFINITION_FORMATION('',$,#35331);
#35223=PRODUCT_DEFINITION_FORMATION('',$,#35332);
#35224=PRODUCT_DEFINITION_FORMATION('',$,#35333);
#35225=PRODUCT_DEFINITION_FORMATION('',$,#35334);
#35226=PRODUCT_DEFINITION_FORMATION('',$,#35335);
#35227=PRODUCT_DEFINITION_FORMATION('',$,#35336);
#35228=PRODUCT_DEFINITION_FORMATION('',$,#35337);
#35229=PRODUCT_DEFINITION_FORMATION('',$,#35338);
#35230=PRODUCT_DEFINITION_FORMATION('',$,#35339);
#35231=PRODUCT_DEFINITION_FORMATION('',$,#35340);
#35232=PRODUCT_DEFINITION_FORMATION('',$,#35341);
#35233=PRODUCT_RELATED_PRODUCT_CATEGORY('PAT-085','PAT-085',(#35289));
#35234=PRODUCT_RELATED_PRODUCT_CATEGORY(
'Extrusion frame and pinion bearings',
'Extrusion frame and pinion bearings',(#35290));
#35235=PRODUCT_RELATED_PRODUCT_CATEGORY('Base','Base',(#35291));
#35236=PRODUCT_RELATED_PRODUCT_CATEGORY('Foot strip','Foot strip',(#35292));
#35237=PRODUCT_RELATED_PRODUCT_CATEGORY('Foot strip (1)',
'Foot strip (1)',(#35293));
#35238=PRODUCT_RELATED_PRODUCT_CATEGORY('Rail support plate',
'Rail support plate',(#35294));
#35239=PRODUCT_RELATED_PRODUCT_CATEGORY('End stop','End stop',(#35295));
#35240=PRODUCT_RELATED_PRODUCT_CATEGORY('End bumper','End bumper',(#35296));
#35241=PRODUCT_RELATED_PRODUCT_CATEGORY('End stop (1)','End stop (1)',(#35297));
#35242=PRODUCT_RELATED_PRODUCT_CATEGORY('End bumper (1)',
'End bumper (1)',(#35298));
#35243=PRODUCT_RELATED_PRODUCT_CATEGORY('Pinion bearing pedestal',
'Pinion bearing pedestal',(#35299));
#35244=PRODUCT_RELATED_PRODUCT_CATEGORY('Bearing cap','Bearing cap',(#35300));
#35245=PRODUCT_RELATED_PRODUCT_CATEGORY('Bearing cap (1)',
'Bearing cap (1)',(#35301));
#35246=PRODUCT_RELATED_PRODUCT_CATEGORY('Pinion bearing pedestal (1)',
'Pinion bearing pedestal (1)',(#35302));
#35247=PRODUCT_RELATED_PRODUCT_CATEGORY('Bearing cap (2)',
'Bearing cap (2)',(#35303));
#35248=PRODUCT_RELATED_PRODUCT_CATEGORY('Bearing cap (3)',
'Bearing cap (3)',(#35304));
#35249=PRODUCT_RELATED_PRODUCT_CATEGORY(
'Slotted Extrusion - 20 x 20 x 200 mm',
'Slotted Extrusion - 20 x 20 x 200 mm',(#35305));
#35250=PRODUCT_RELATED_PRODUCT_CATEGORY('Captive slot nut',
'Captive slot nut',(#35306));
#35251=PRODUCT_RELATED_PRODUCT_CATEGORY('Flat Washer - M5',
'Flat Washer - M5',(#35307));
#35252=PRODUCT_RELATED_PRODUCT_CATEGORY(
'Linear Guide Rail - 15 mm, 220 mm Long',
'Linear Guide Rail - 15 mm, 220 mm Long',(#35308));
#35253=PRODUCT_RELATED_PRODUCT_CATEGORY('Cap Screw - M5x20',
'Cap Screw - M5x20',(#35309));
#35254=PRODUCT_RELATED_PRODUCT_CATEGORY(
'Sealed Ball Bearing - 12 x 32 x 10 mm',
'Sealed Ball Bearing - 12 x 32 x 10 mm',(#35310));
#35255=PRODUCT_RELATED_PRODUCT_CATEGORY('Inner ring','Inner ring',(#35311));
#35256=PRODUCT_RELATED_PRODUCT_CATEGORY('Outer ring','Outer ring',(#35312));
#35257=PRODUCT_RELATED_PRODUCT_CATEGORY('Balls','Balls',(#35313));
#35258=PRODUCT_RELATED_PRODUCT_CATEGORY('Cage','Cage',(#35314));
#35259=PRODUCT_RELATED_PRODUCT_CATEGORY('Seals 2RS','Seals 2RS',(#35315));
#35260=PRODUCT_RELATED_PRODUCT_CATEGORY('M4x10 Cap Screw',
'M4x10 Cap Screw',(#35316));
#35261=PRODUCT_RELATED_PRODUCT_CATEGORY('Rack and carriage',
'Rack and carriage',(#35317));
#35262=PRODUCT_RELATED_PRODUCT_CATEGORY('Table','Table',(#35318));
#35263=PRODUCT_RELATED_PRODUCT_CATEGORY('Module 2 rack','Module 2 rack',
(#35319));
#35264=PRODUCT_RELATED_PRODUCT_CATEGORY(
'Flanged Linear Guide Carriage - 15 mm',
'Flanged Linear Guide Carriage - 15 mm',(#35320));
#35265=PRODUCT_RELATED_PRODUCT_CATEGORY('Block','Block',(#35321));
#35266=PRODUCT_RELATED_PRODUCT_CATEGORY('End cap +','End cap +',(#35322));
#35267=PRODUCT_RELATED_PRODUCT_CATEGORY('End cap','End cap',(#35323));
#35268=PRODUCT_RELATED_PRODUCT_CATEGORY('M5x14 Cap Screw',
'M5x14 Cap Screw',(#35324));
#35269=PRODUCT_RELATED_PRODUCT_CATEGORY('Pinion shaft and crank',
'Pinion shaft and crank',(#35325));
#35270=PRODUCT_RELATED_PRODUCT_CATEGORY('Pinion shaft','Pinion shaft',(#35326));
#35271=PRODUCT_RELATED_PRODUCT_CATEGORY('Gear front spacer',
'Gear front spacer',(#35327));
#35272=PRODUCT_RELATED_PRODUCT_CATEGORY('Rear inner spacer',
'Rear inner spacer',(#35328));
#35273=PRODUCT_RELATED_PRODUCT_CATEGORY('Crank inner spacer',
'Crank inner spacer',(#35329));
#35274=PRODUCT_RELATED_PRODUCT_CATEGORY('Shaft keeper','Shaft keeper',(#35330));
#35275=PRODUCT_RELATED_PRODUCT_CATEGORY('Shaft keeper (1)',
'Shaft keeper (1)',(#35331));
#35276=PRODUCT_RELATED_PRODUCT_CATEGORY('Rear end sleeve',
'Rear end sleeve',(#35332));
#35277=PRODUCT_RELATED_PRODUCT_CATEGORY('Crank','Crank',(#35333));
#35278=PRODUCT_RELATED_PRODUCT_CATEGORY('Grip bushing','Grip bushing',(#35334));
#35279=PRODUCT_RELATED_PRODUCT_CATEGORY(
'Spur Gear - Module 2, 20 Teeth, 12 mm Bore',
'Spur Gear - Module 2, 20 Teeth, 12 mm Bore',(#35335));
#35280=PRODUCT_RELATED_PRODUCT_CATEGORY('Cap Screw - M4x16',
'Cap Screw - M4x16',(#35336));
#35281=PRODUCT_RELATED_PRODUCT_CATEGORY('Key 4x4x14','Key 4x4x14',(#35337));
#35282=PRODUCT_RELATED_PRODUCT_CATEGORY('Flat Washer - M6',
'Flat Washer - M6',(#35338));
#35283=PRODUCT_RELATED_PRODUCT_CATEGORY('Cap Screw - M6x25',
'Cap Screw - M6x25',(#35339));
#35284=PRODUCT_RELATED_PRODUCT_CATEGORY('Revolving grip',
'Revolving grip',(#35340));
#35285=PRODUCT_RELATED_PRODUCT_CATEGORY('Handle','Handle',(#35341));
#35286=APPLICATION_PROTOCOL_DEFINITION('international standard',
'automotive_design',2009,#35287);
#35287=APPLICATION_CONTEXT(
'Core Data for Automotive Mechanical Design Process');
#35288=PRODUCT_CONTEXT('part definition',#35287,'mechanical');
#35289=PRODUCT('PAT-085','PAT-085',
'PAT-085',(#35288));
#35290=PRODUCT('Extrusion frame and pinion bearings',
'Extrusion frame and pinion bearings',
'Extrusion frame and pinion bearings',(#35288));
#35291=PRODUCT('Base','Base','Base',(#35288));
#35292=PRODUCT('Foot strip','Foot strip','Foot strip',(#35288));
#35293=PRODUCT('Foot strip (1)','Foot strip (1)','Foot strip (1)',(#35288));
#35294=PRODUCT('Rail support plate','Rail support plate',
'Rail support plate',(#35288));
#35295=PRODUCT('End stop','End stop','End stop',(#35288));
#35296=PRODUCT('End bumper','End bumper','End bumper',(#35288));
#35297=PRODUCT('End stop (1)','End stop (1)','End stop (1)',(#35288));
#35298=PRODUCT('End bumper (1)','End bumper (1)','End bumper (1)',(#35288));
#35299=PRODUCT('Pinion bearing pedestal','Pinion bearing pedestal',
'Pinion bearing pedestal',(#35288));
#35300=PRODUCT('Bearing cap','Bearing cap','Bearing cap',(#35288));
#35301=PRODUCT('Bearing cap (1)','Bearing cap (1)','Bearing cap (1)',(#35288));
#35302=PRODUCT('Pinion bearing pedestal (1)',
'Pinion bearing pedestal (1)','Pinion bearing pedestal (1)',(#35288));
#35303=PRODUCT('Bearing cap (2)','Bearing cap (2)','Bearing cap (2)',(#35288));
#35304=PRODUCT('Bearing cap (3)','Bearing cap (3)','Bearing cap (3)',(#35288));
#35305=PRODUCT('Slotted Extrusion - 20 x 20 x 200 mm',
'Slotted Extrusion - 20 x 20 x 200 mm',
'Slotted Extrusion - 20 x 20 x 200 mm',(#35288));
#35306=PRODUCT('Captive slot nut','Captive slot nut','Captive slot nut',
(#35288));
#35307=PRODUCT('Flat Washer - M5','Flat Washer - M5','Flat Washer - M5',
(#35288));
#35308=PRODUCT('Linear Guide Rail - 15 mm, 220 mm Long',
'Linear Guide Rail - 15 mm, 220 mm Long',
'Linear Guide Rail - 15 mm, 220 mm Long',(#35288));
#35309=PRODUCT('Cap Screw - M5x20','Cap Screw - M5x20',
'Cap Screw - M5x20',(#35288));
#35310=PRODUCT('Sealed Ball Bearing - 12 x 32 x 10 mm',
'Sealed Ball Bearing - 12 x 32 x 10 mm',
'Sealed Ball Bearing - 12 x 32 x 10 mm',(#35288));
#35311=PRODUCT('Inner ring','Inner ring','Inner ring',(#35288));
#35312=PRODUCT('Outer ring','Outer ring','Outer ring',(#35288));
#35313=PRODUCT('Balls','Balls','Balls',(#35288));
#35314=PRODUCT('Cage','Cage','Cage',(#35288));
#35315=PRODUCT('Seals 2RS','Seals 2RS','Seals 2RS',(#35288));
#35316=PRODUCT('M4x10 Cap Screw','M4x10 Cap Screw','M4x10 Cap Screw',(#35288));
#35317=PRODUCT('Rack and carriage','Rack and carriage',
'Rack and carriage',(#35288));
#35318=PRODUCT('Table','Table','Table',(#35288));
#35319=PRODUCT('Module 2 rack','Module 2 rack','Module 2 rack',(#35288));
#35320=PRODUCT('Flanged Linear Guide Carriage - 15 mm',
'Flanged Linear Guide Carriage - 15 mm',
'Flanged Linear Guide Carriage - 15 mm',(#35288));
#35321=PRODUCT('Block','Block','Block',(#35288));
#35322=PRODUCT('End cap +','End cap +','End cap +',(#35288));
#35323=PRODUCT('End cap','End cap','End cap',(#35288));
#35324=PRODUCT('M5x14 Cap Screw','M5x14 Cap Screw','M5x14 Cap Screw',(#35288));
#35325=PRODUCT('Pinion shaft and crank','Pinion shaft and crank',
'Pinion shaft and crank',(#35288));
#35326=PRODUCT('Pinion shaft','Pinion shaft','Pinion shaft',(#35288));
#35327=PRODUCT('Gear front spacer','Gear front spacer',
'Gear front spacer',(#35288));
#35328=PRODUCT('Rear inner spacer','Rear inner spacer',
'Rear inner spacer',(#35288));
#35329=PRODUCT('Crank inner spacer','Crank inner spacer',
'Crank inner spacer',(#35288));
#35330=PRODUCT('Shaft keeper','Shaft keeper','Shaft keeper',(#35288));
#35331=PRODUCT('Shaft keeper (1)','Shaft keeper (1)','Shaft keeper (1)',(#35288));
#35332=PRODUCT('Rear end sleeve','Rear end sleeve','Rear end sleeve',(#35288));
#35333=PRODUCT('Crank','Crank','Crank',(#35288));
#35334=PRODUCT('Grip bushing','Grip bushing','Grip bushing',(#35288));
#35335=PRODUCT('Spur Gear - Module 2, 20 Teeth, 12 mm Bore',
'Spur Gear - Module 2, 20 Teeth, 12 mm Bore',
'Spur Gear - Module 2, 20 Teeth, 12 mm Bore',(#35288));
#35336=PRODUCT('Cap Screw - M4x16','Cap Screw - M4x16',
'Cap Screw - M4x16',(#35288));
#35337=PRODUCT('Key 4x4x14','Key 4x4x14','Key 4x4x14',(#35288));
#35338=PRODUCT('Flat Washer - M6','Flat Washer - M6','Flat Washer - M6',
(#35288));
#35339=PRODUCT('Cap Screw - M6x25','Cap Screw - M6x25',
'Cap Screw - M6x25',(#35288));
#35340=PRODUCT('Revolving grip','Revolving grip','Revolving grip',(#35288));
#35341=PRODUCT('Handle','Handle','Handle',(#35288));
#35342=PRESENTATION_STYLE_ASSIGNMENT((#35348));
#35343=PRESENTATION_STYLE_ASSIGNMENT((#35349));
#35344=PRESENTATION_STYLE_ASSIGNMENT((#35350));
#35345=PRESENTATION_STYLE_ASSIGNMENT((#35351));
#35346=PRESENTATION_STYLE_ASSIGNMENT((#35352));
#35347=PRESENTATION_STYLE_ASSIGNMENT((#35353));
#35348=SURFACE_STYLE_USAGE(.BOTH.,#35354);
#35349=SURFACE_STYLE_USAGE(.BOTH.,#35355);
#35350=SURFACE_STYLE_USAGE(.BOTH.,#35356);
#35351=SURFACE_STYLE_USAGE(.BOTH.,#35357);
#35352=SURFACE_STYLE_USAGE(.BOTH.,#35358);
#35353=SURFACE_STYLE_USAGE(.BOTH.,#35359);
#35354=SURFACE_SIDE_STYLE('',(#35360));
#35355=SURFACE_SIDE_STYLE('',(#35361));
#35356=SURFACE_SIDE_STYLE('',(#35362));
#35357=SURFACE_SIDE_STYLE('',(#35363));
#35358=SURFACE_SIDE_STYLE('',(#35364));
#35359=SURFACE_SIDE_STYLE('',(#35365));
#35360=SURFACE_STYLE_FILL_AREA(#35366);
#35361=SURFACE_STYLE_FILL_AREA(#35367);
#35362=SURFACE_STYLE_FILL_AREA(#35368);
#35363=SURFACE_STYLE_FILL_AREA(#35369);
#35364=SURFACE_STYLE_FILL_AREA(#35370);
#35365=SURFACE_STYLE_FILL_AREA(#35371);
#35366=FILL_AREA_STYLE('Steel - Satin',(#35372));
#35367=FILL_AREA_STYLE('CAD Library Painted - Deep blue',(#35373));
#35368=FILL_AREA_STYLE('CAD Library Painted - Steel gray',(#35374));
#35369=FILL_AREA_STYLE('CAD Library Painted - Engineering blue',(#35375));
#35370=FILL_AREA_STYLE('CAD Library Painted - Graphite',(#35376));
#35371=FILL_AREA_STYLE('CAD Library Painted - Light blue',(#35377));
#35372=FILL_AREA_STYLE_COLOUR('Steel - Satin',#35378);
#35373=FILL_AREA_STYLE_COLOUR('CAD Library Painted - Deep blue',#35379);
#35374=FILL_AREA_STYLE_COLOUR('CAD Library Painted - Steel gray',#35380);
#35375=FILL_AREA_STYLE_COLOUR('CAD Library Painted - Engineering blue',
#35381);
#35376=FILL_AREA_STYLE_COLOUR('CAD Library Painted - Graphite',#35382);
#35377=FILL_AREA_STYLE_COLOUR('CAD Library Painted - Light blue',#35383);
#35378=COLOUR_RGB('Steel - Satin',0.627450980392157,0.627450980392157,0.627450980392157);
#35379=COLOUR_RGB('CAD Library Painted - Deep blue',0.0784313725490196,
0.203921568627451,0.349019607843137);
#35380=COLOUR_RGB('CAD Library Painted - Steel gray',0.592156862745098,
0.631372549019608,0.67843137254902);
#35381=COLOUR_RGB('CAD Library Painted - Engineering blue',0.12156862745098,
0.356862745098039,0.6);
#35382=COLOUR_RGB('CAD Library Painted - Graphite',0.168627450980392,0.192156862745098,
0.231372549019608);
#35383=COLOUR_RGB('CAD Library Painted - Light blue',0.286274509803922,
0.552941176470588,0.780392156862745);
#35384=COLOUR_RGB('Dark Blue',0.08,0.2,0.34);
#35385=FILL_AREA_STYLE_COLOUR('',#35384);
#35386=FILL_AREA_STYLE('',(#35385));
#35387=SURFACE_STYLE_FILL_AREA(#35386);
#35388=SURFACE_SIDE_STYLE('',(#35387));
#35389=SURFACE_STYLE_USAGE(.BOTH.,#35388);
#35390=PRESENTATION_STYLE_ASSIGNMENT((#35389));
#35391=COLOUR_RGB('Light Blue',0.38,0.62,0.78);
#35392=FILL_AREA_STYLE_COLOUR('',#35391);
#35393=FILL_AREA_STYLE('',(#35392));
#35394=SURFACE_STYLE_FILL_AREA(#35393);
#35395=SURFACE_SIDE_STYLE('',(#35394));
#35396=SURFACE_STYLE_USAGE(.BOTH.,#35395);
#35397=PRESENTATION_STYLE_ASSIGNMENT((#35396));
#35398=COLOUR_RGB('Sky Blue',0.24,0.69,0.87);
#35399=FILL_AREA_STYLE_COLOUR('',#35398);
#35400=FILL_AREA_STYLE('',(#35399));
#35401=SURFACE_STYLE_FILL_AREA(#35400);
#35402=SURFACE_SIDE_STYLE('',(#35401));
#35403=SURFACE_STYLE_USAGE(.BOTH.,#35402);
#35404=PRESENTATION_STYLE_ASSIGNMENT((#35403));
#35405=COLOUR_RGB('Grey',0.48,0.52,0.57);
#35406=FILL_AREA_STYLE_COLOUR('',#35405);
#35407=FILL_AREA_STYLE('',(#35406));
#35408=SURFACE_STYLE_FILL_AREA(#35407);
#35409=SURFACE_SIDE_STYLE('',(#35408));
#35410=SURFACE_STYLE_USAGE(.BOTH.,#35409);
#35411=PRESENTATION_STYLE_ASSIGNMENT((#35410));
#35412=COLOUR_RGB('Black',0.12,0.14,0.17);
#35413=FILL_AREA_STYLE_COLOUR('',#35412);
#35414=FILL_AREA_STYLE('',(#35413));
#35415=SURFACE_STYLE_FILL_AREA(#35414);
#35416=SURFACE_SIDE_STYLE('',(#35415));
#35417=SURFACE_STYLE_USAGE(.BOTH.,#35416);
#35418=PRESENTATION_STYLE_ASSIGNMENT((#35417));
#35419=COLOUR_RGB('Off White',0.89,0.88,0.83);
#35420=FILL_AREA_STYLE_COLOUR('',#35419);
#35421=FILL_AREA_STYLE('',(#35420));
#35422=SURFACE_STYLE_FILL_AREA(#35421);
#35423=SURFACE_SIDE_STYLE('',(#35422));
#35424=SURFACE_STYLE_USAGE(.BOTH.,#35423);
#35425=PRESENTATION_STYLE_ASSIGNMENT((#35424));
ENDSEC;
END-ISO-10303-21;
